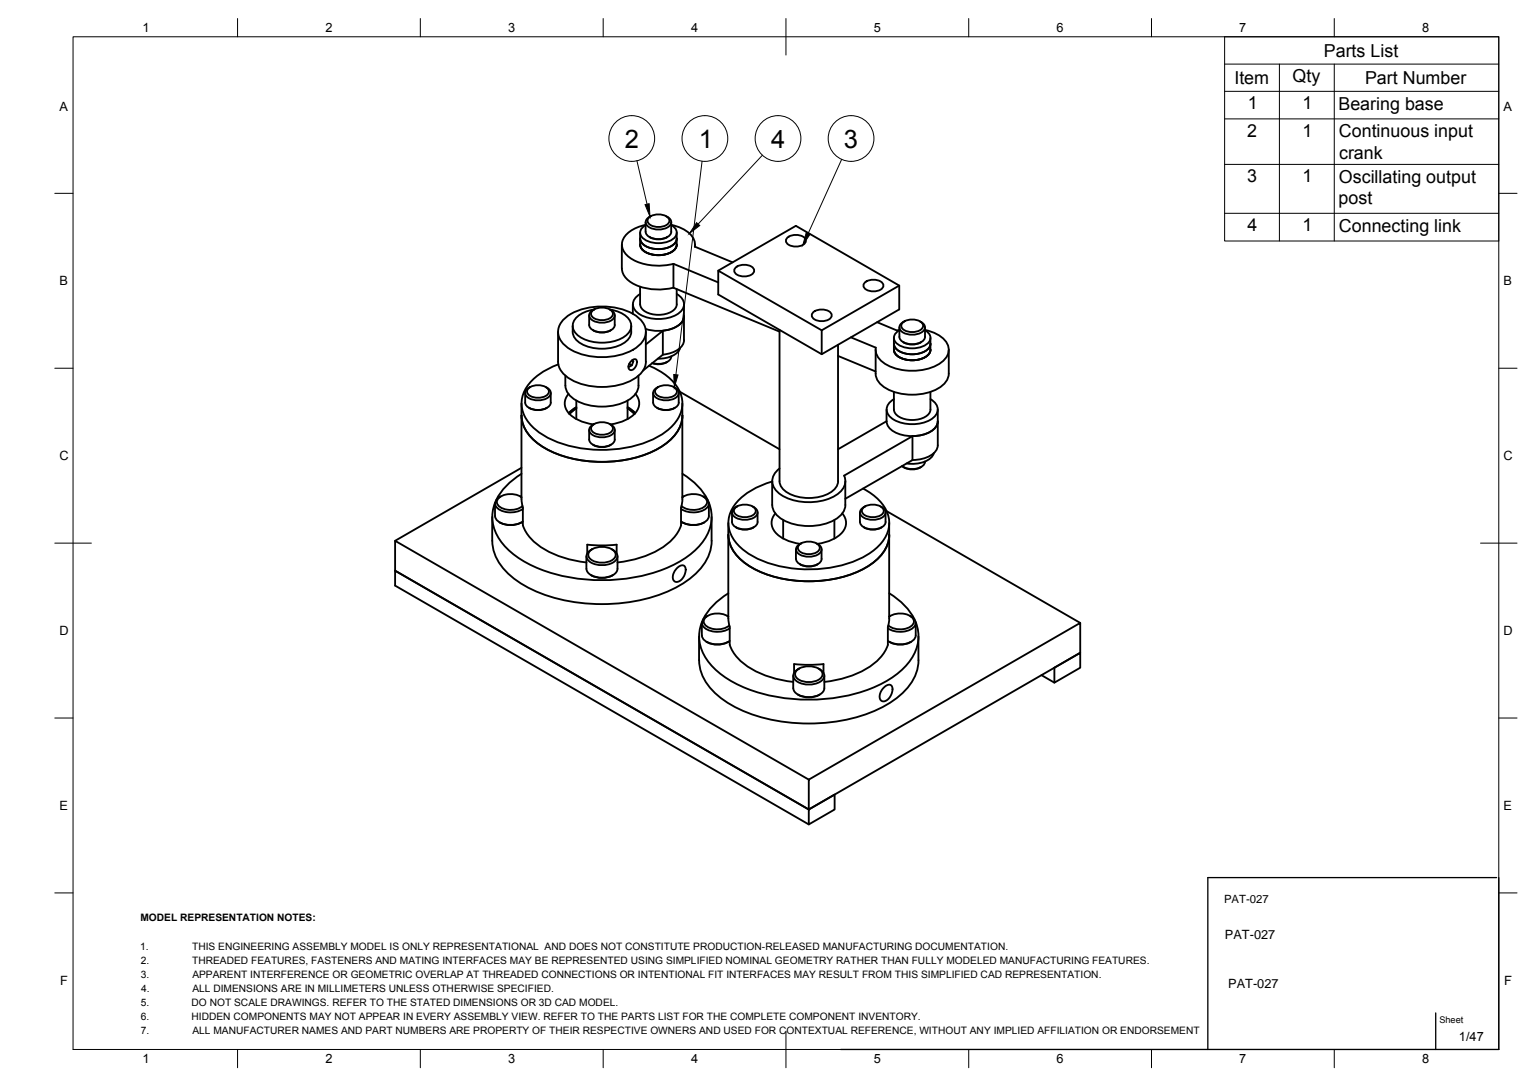
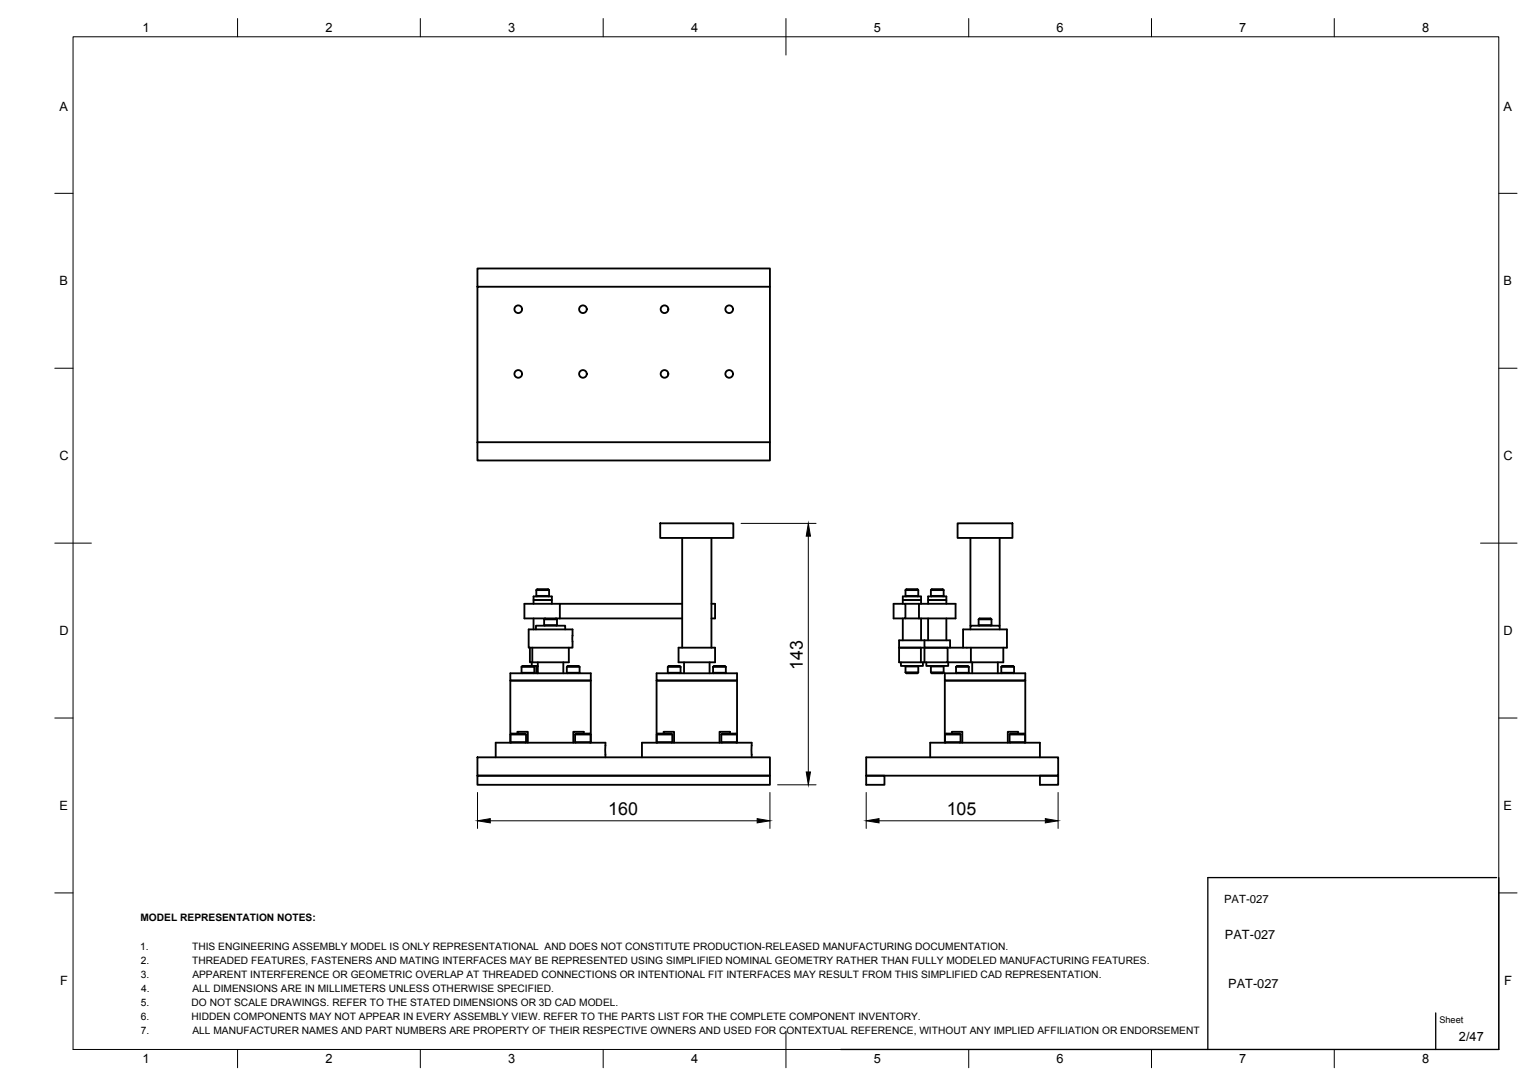
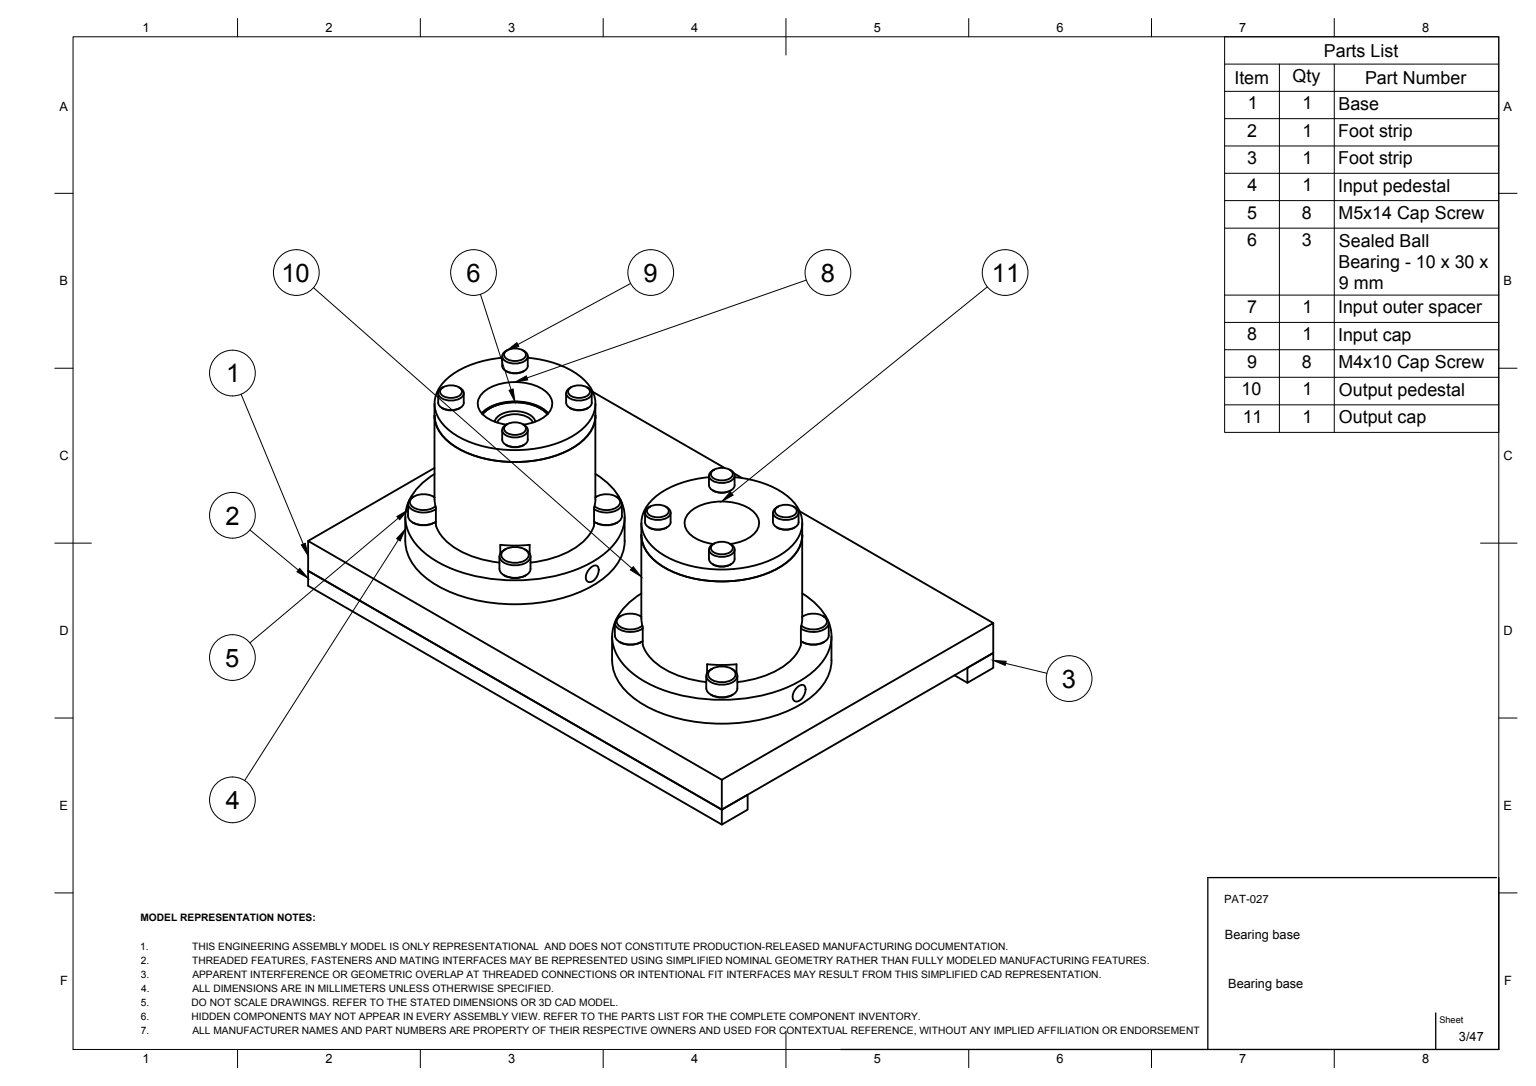
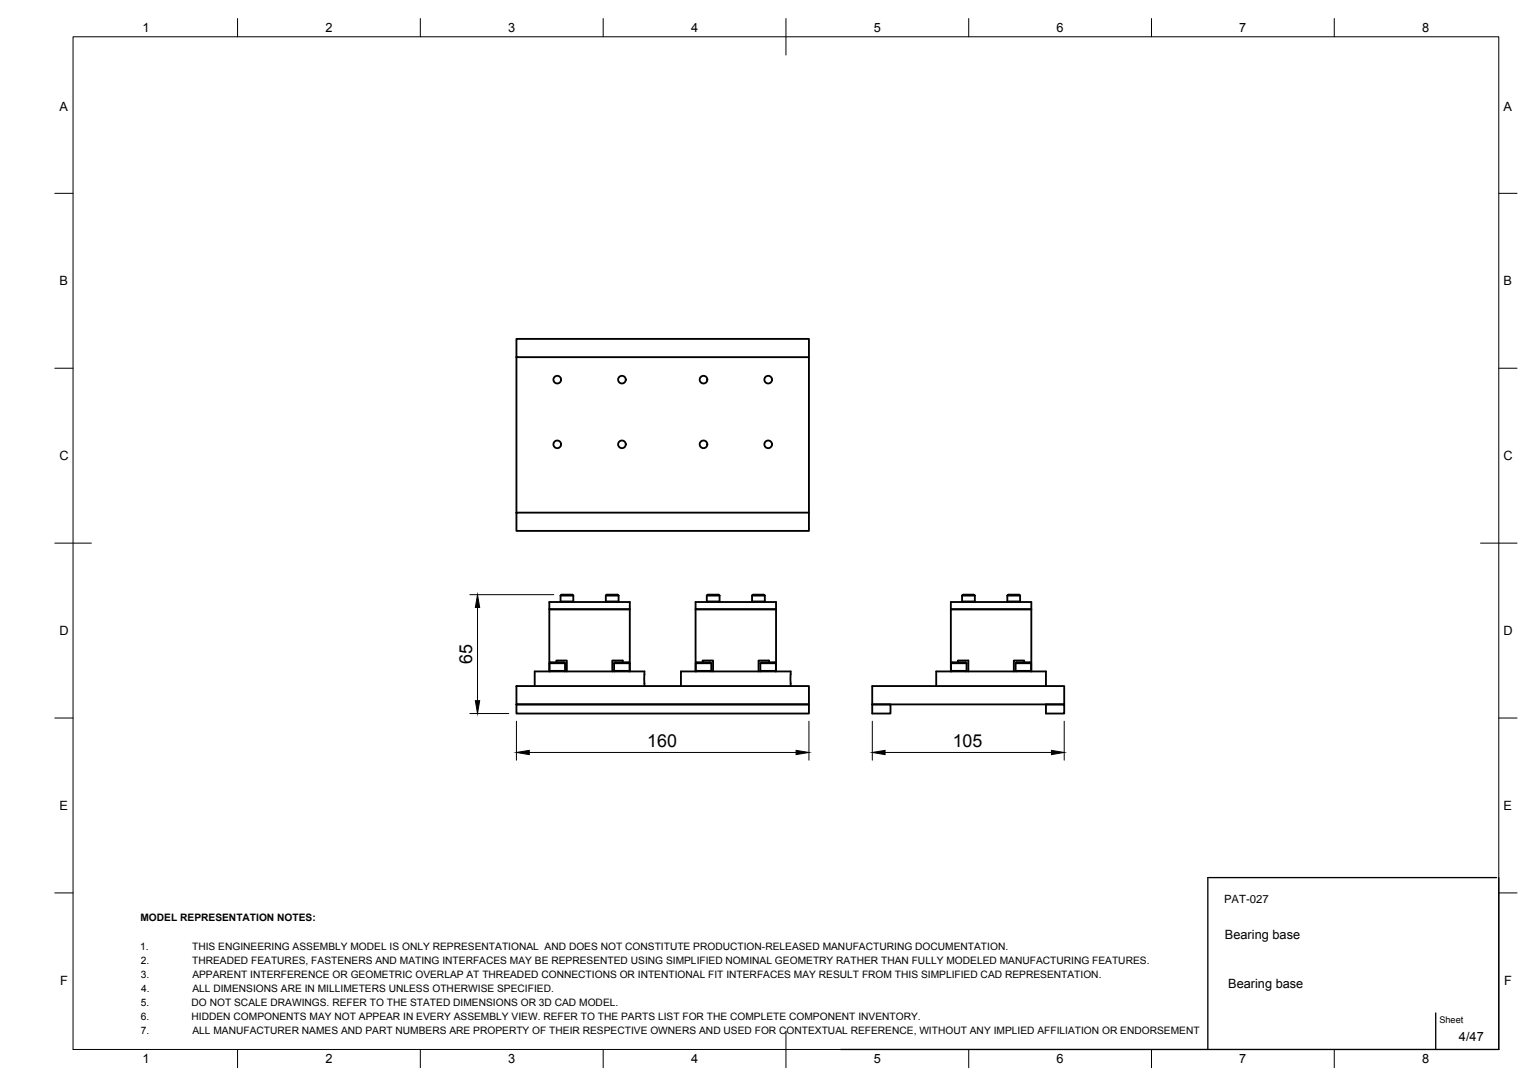
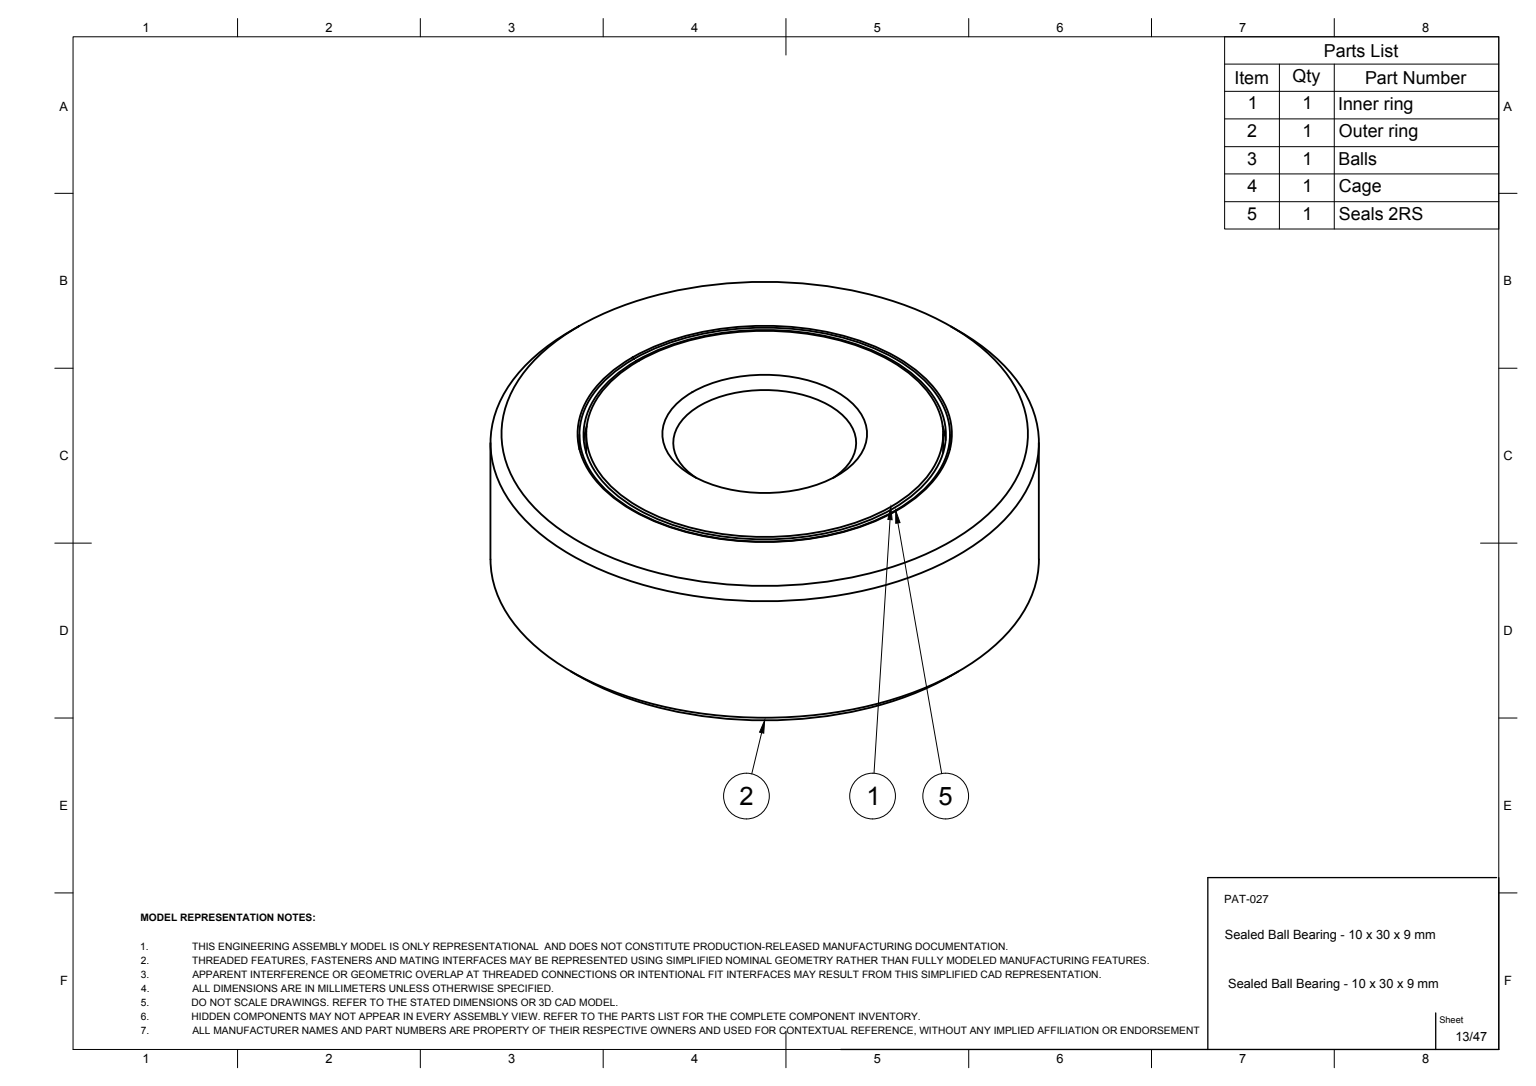
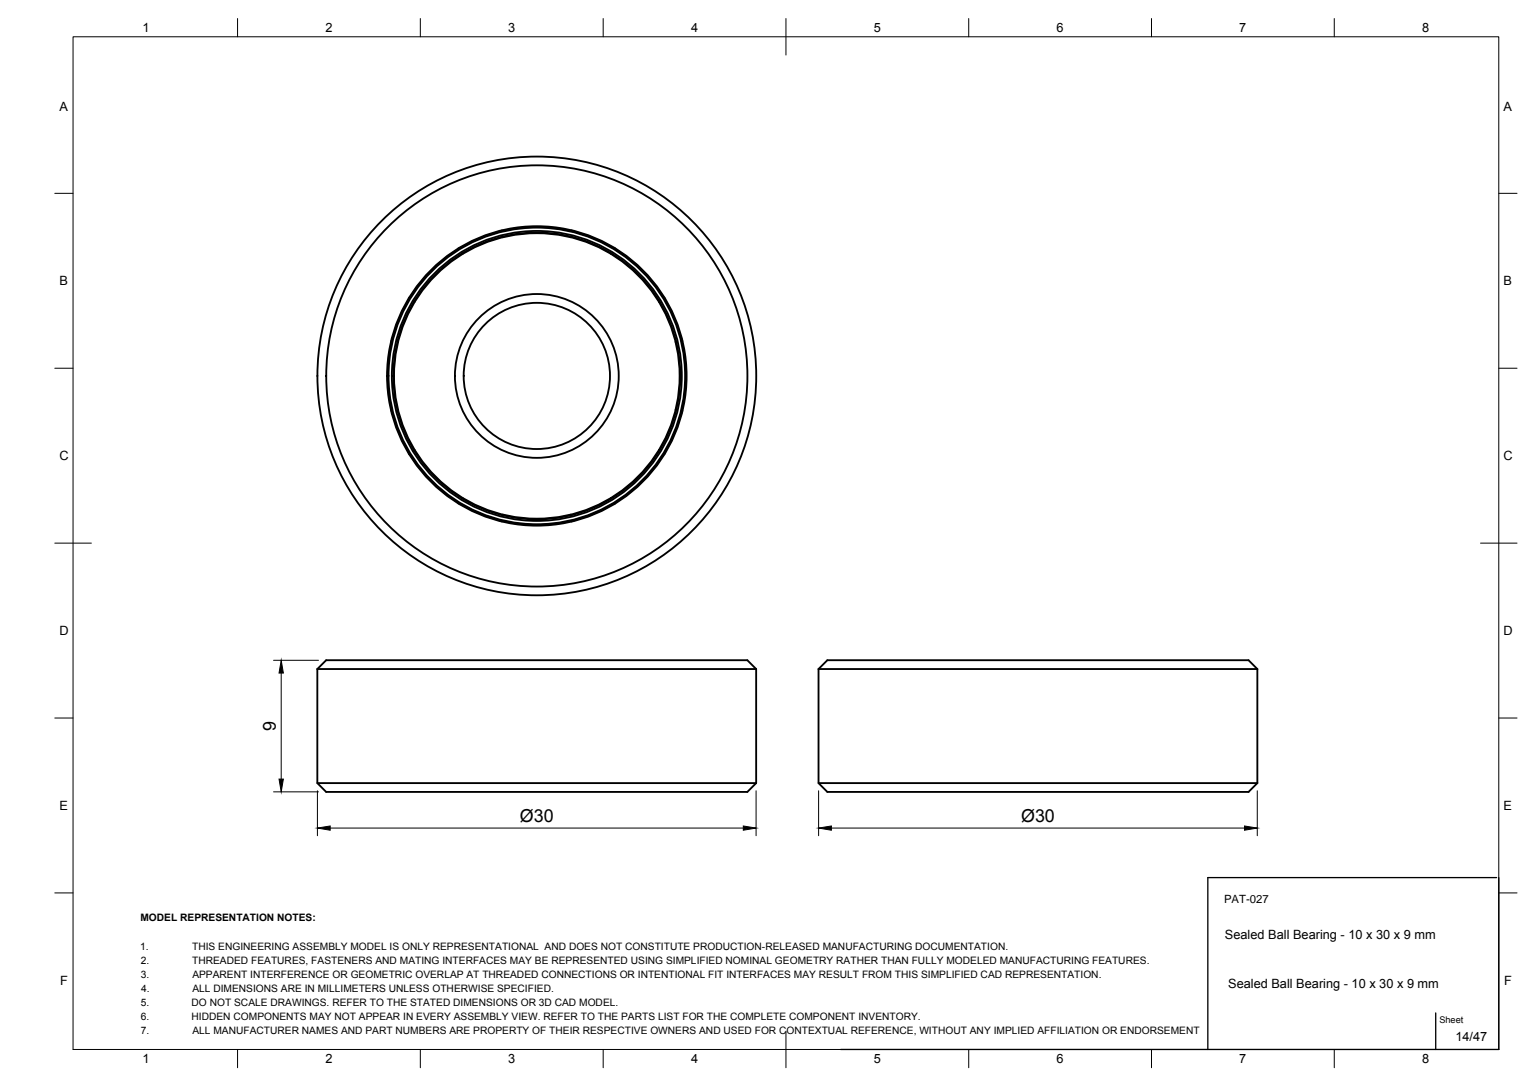
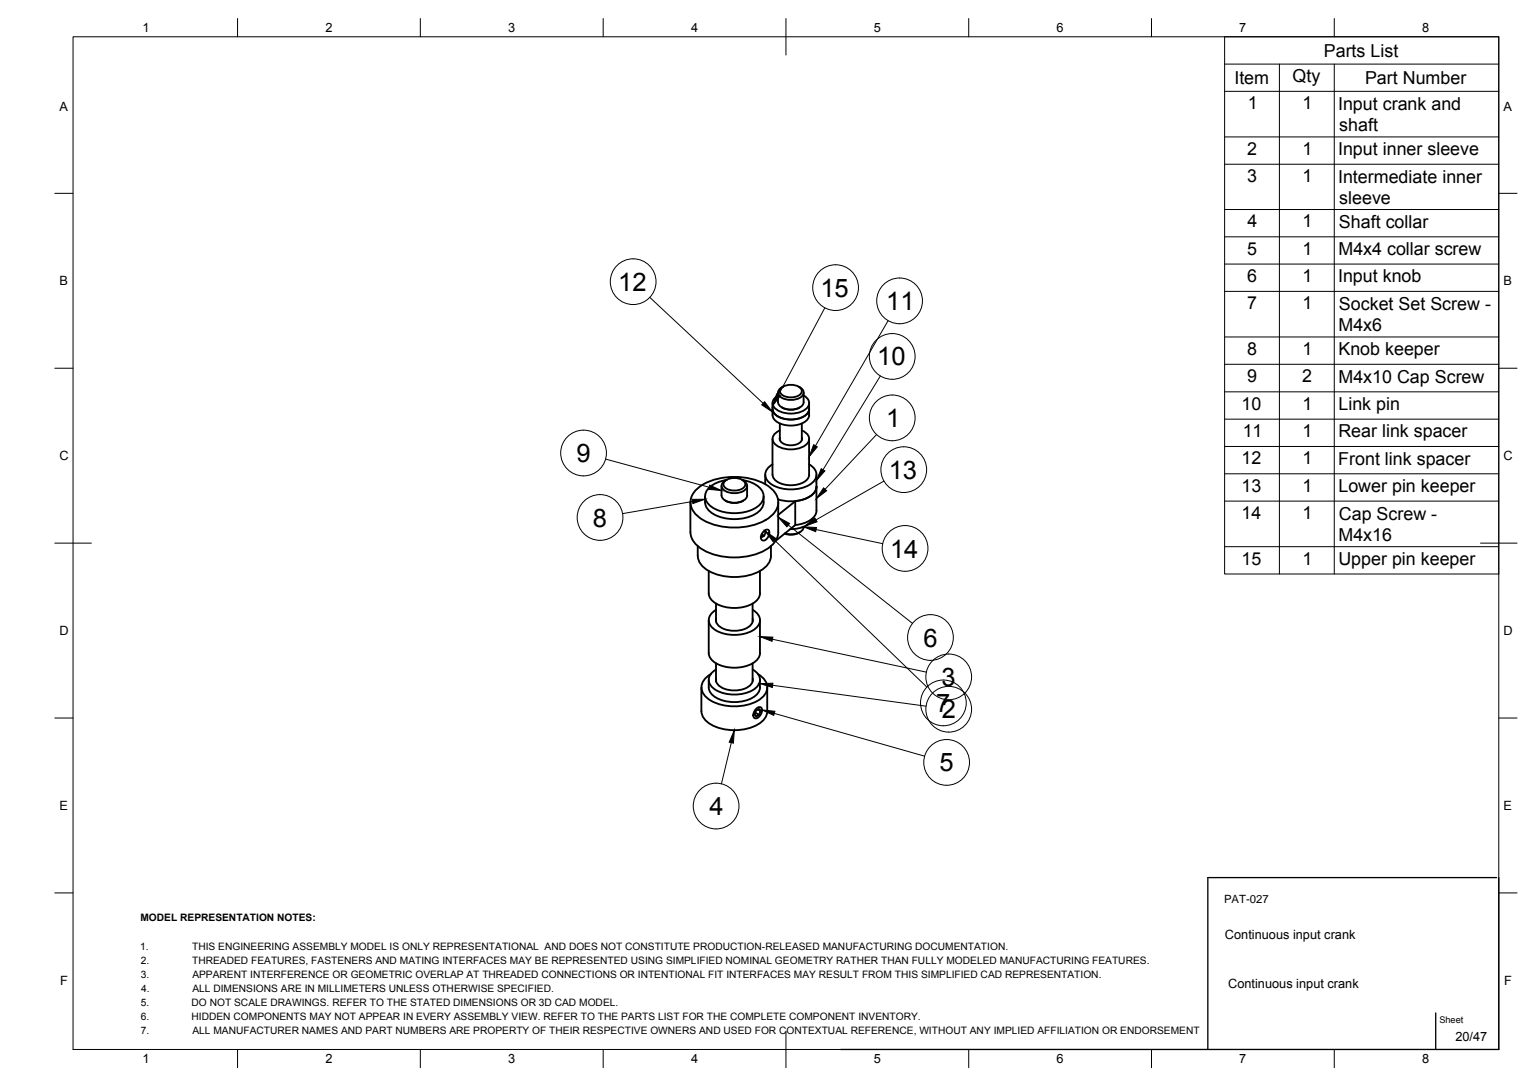
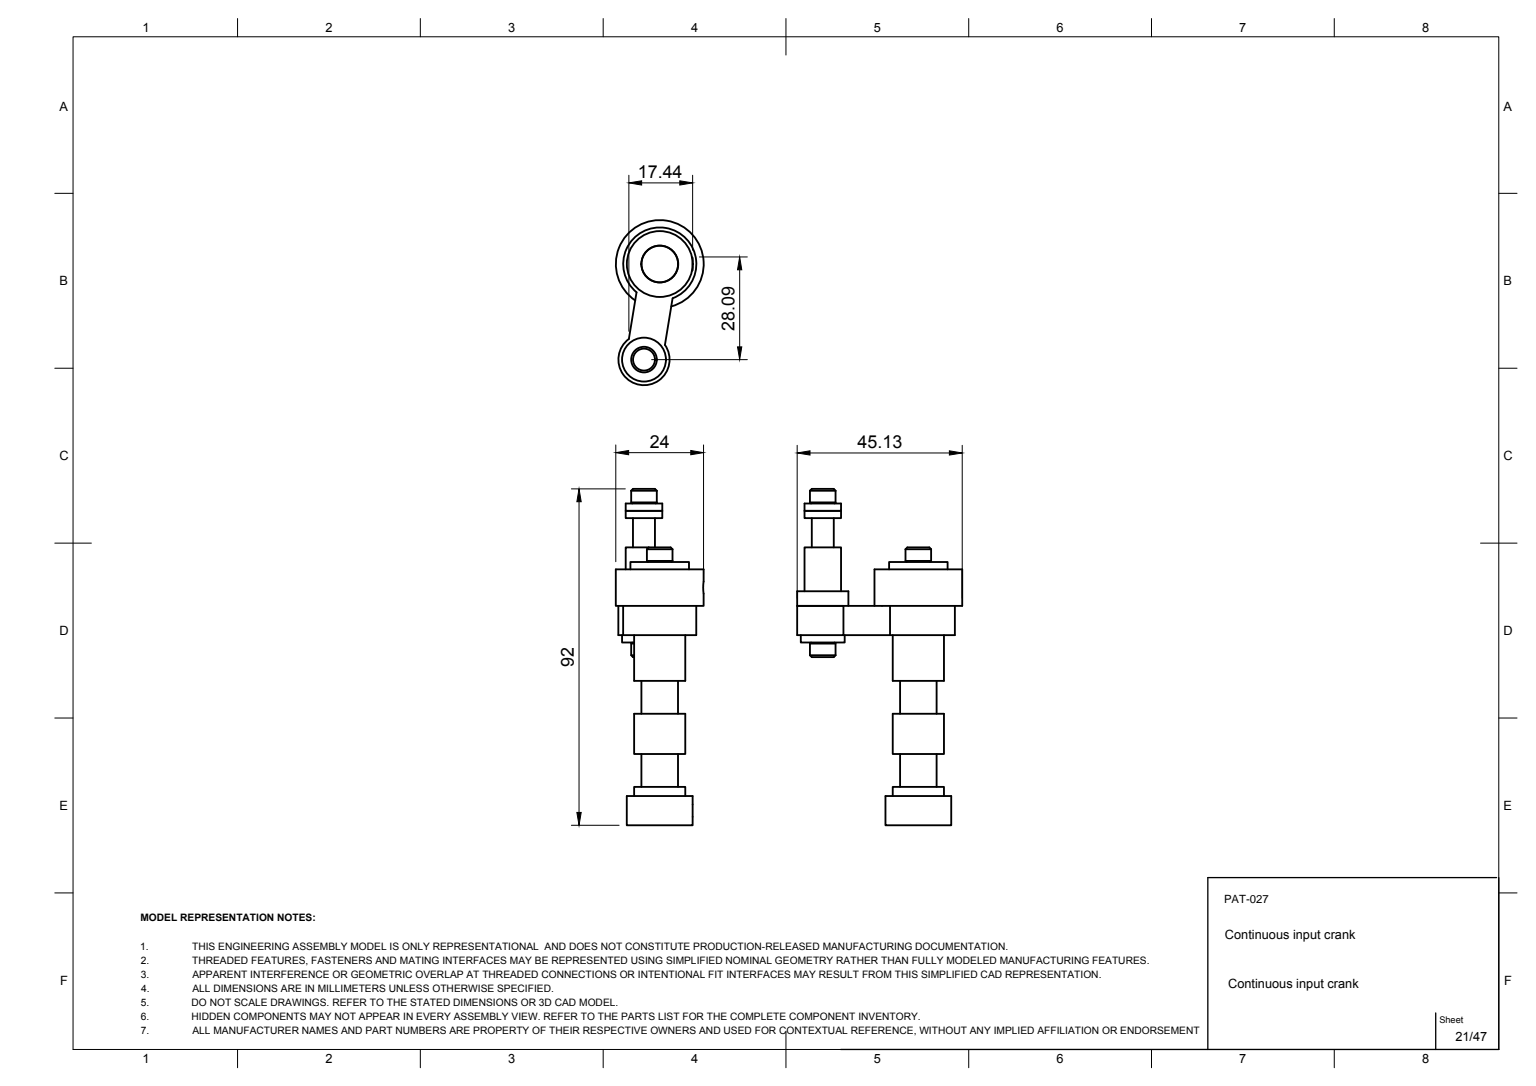
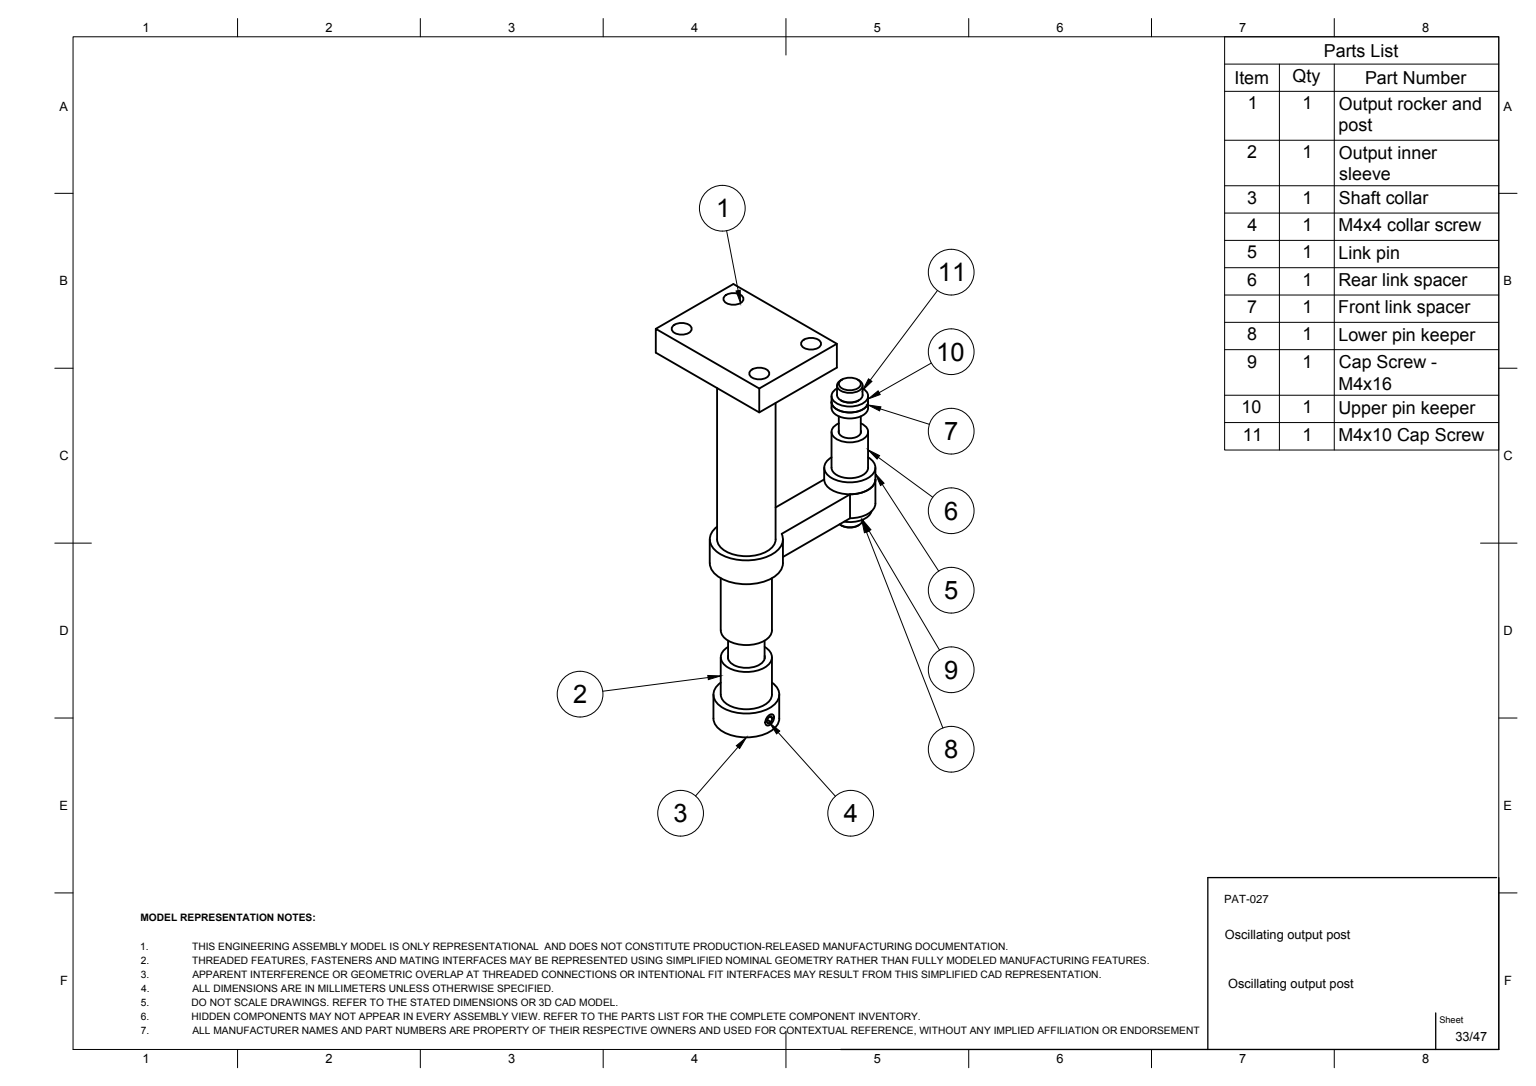
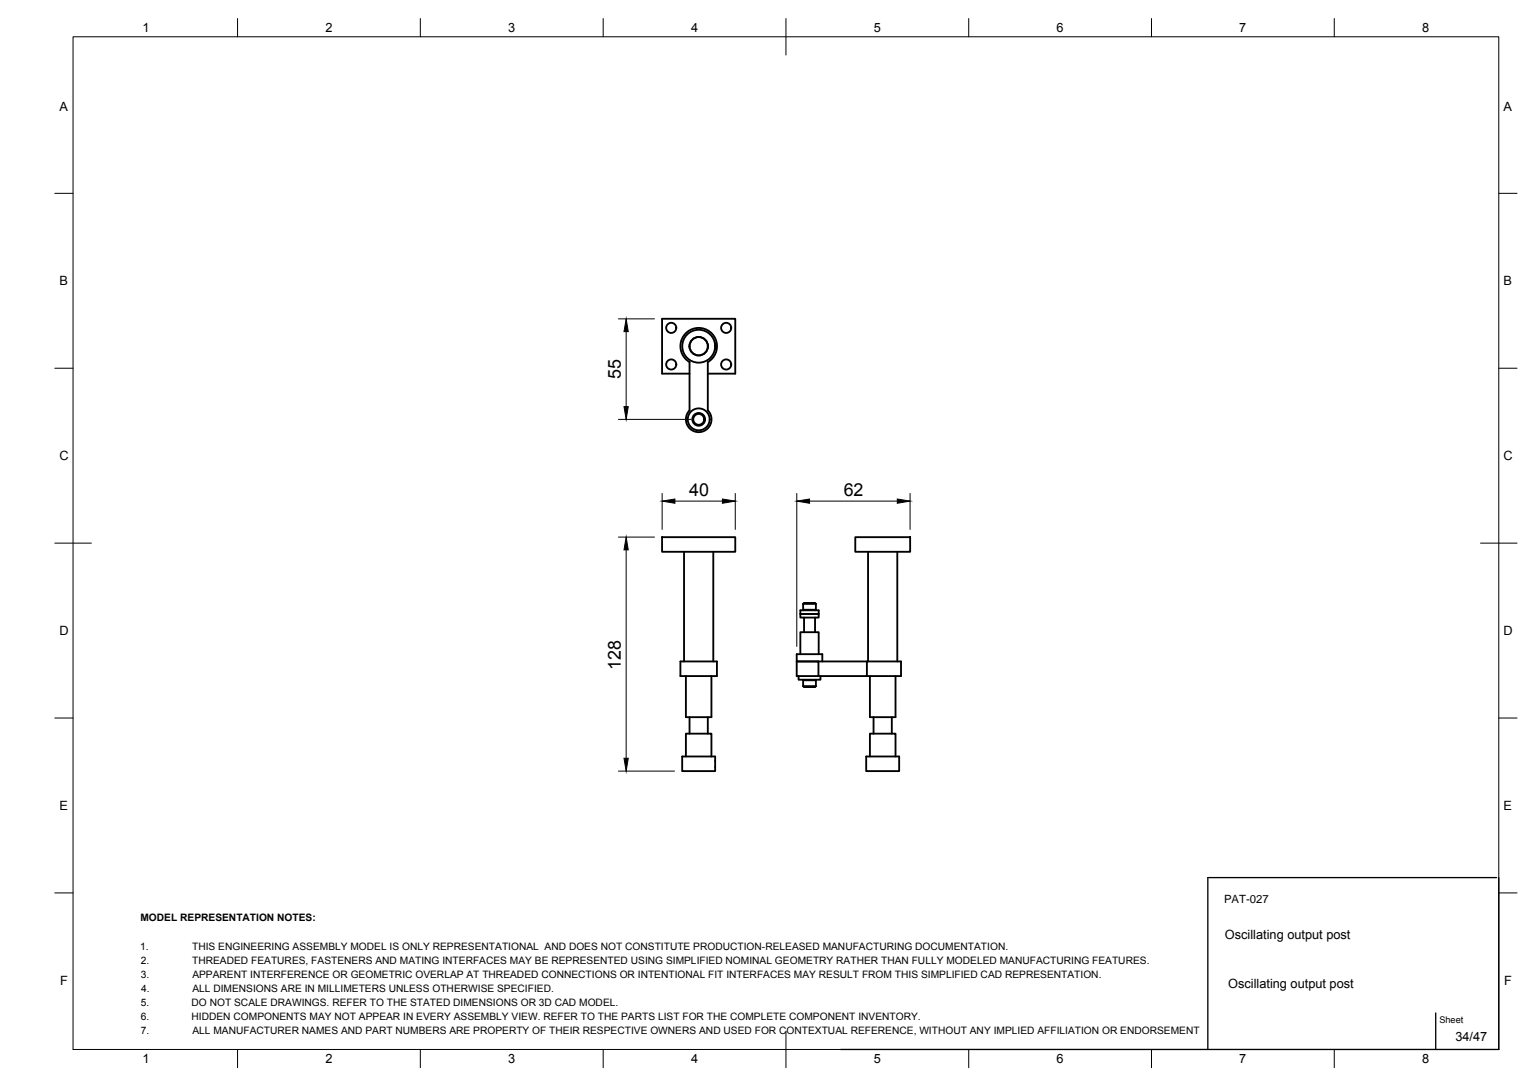
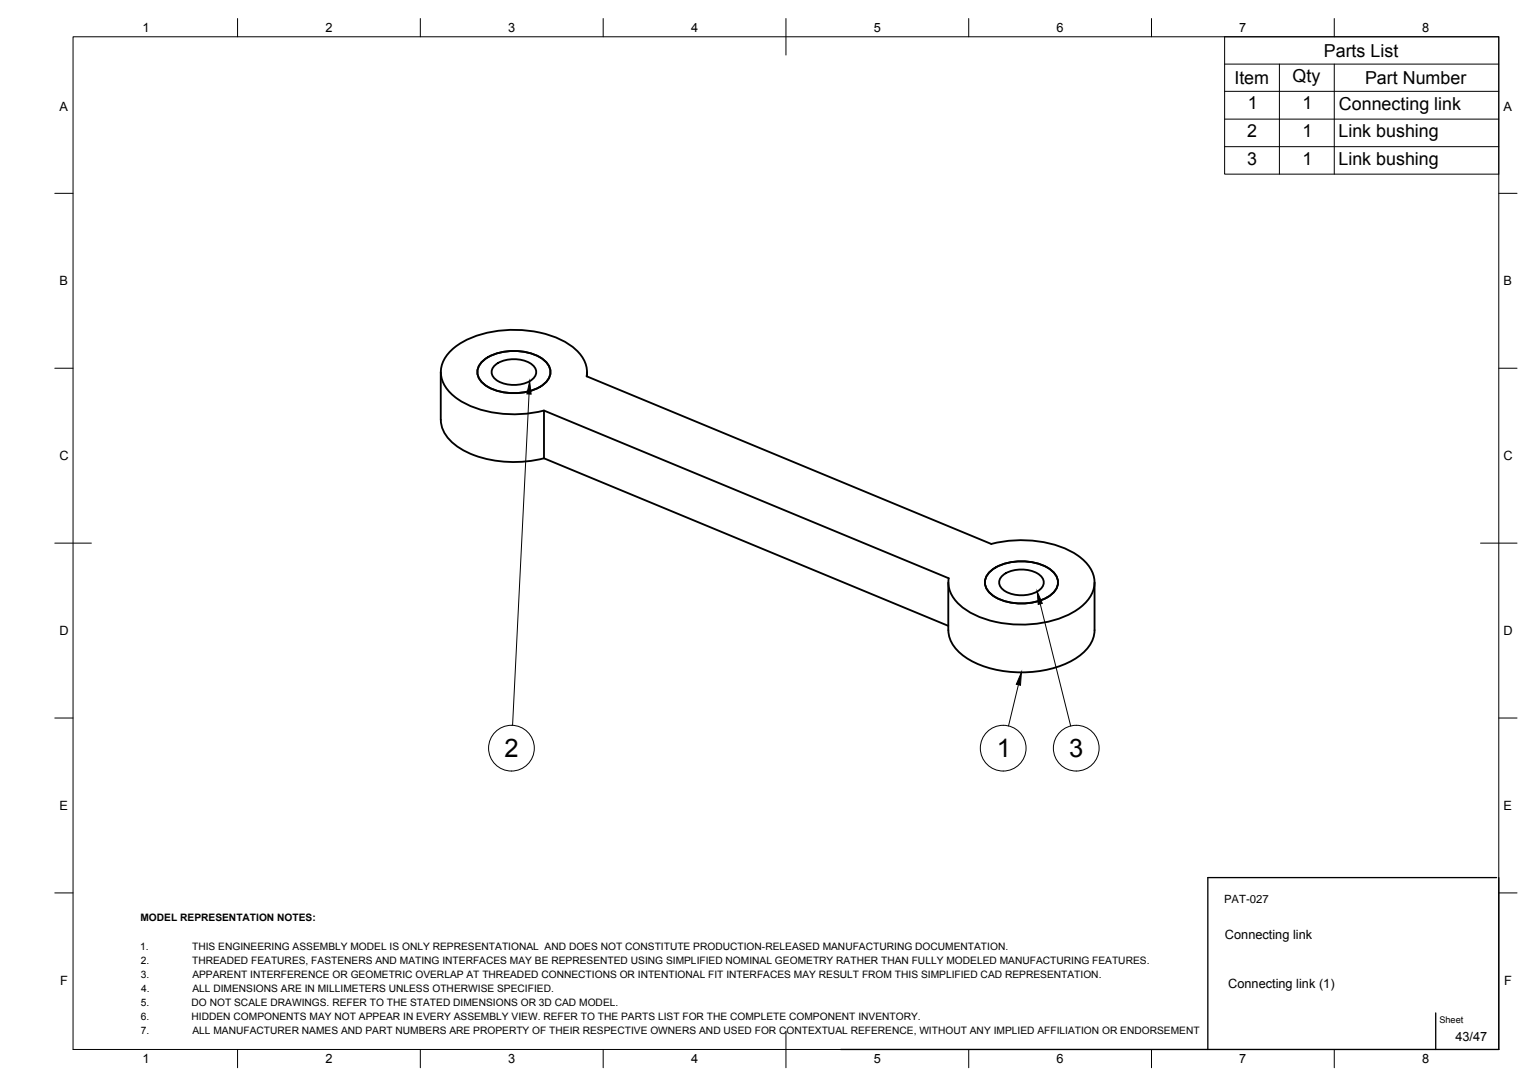
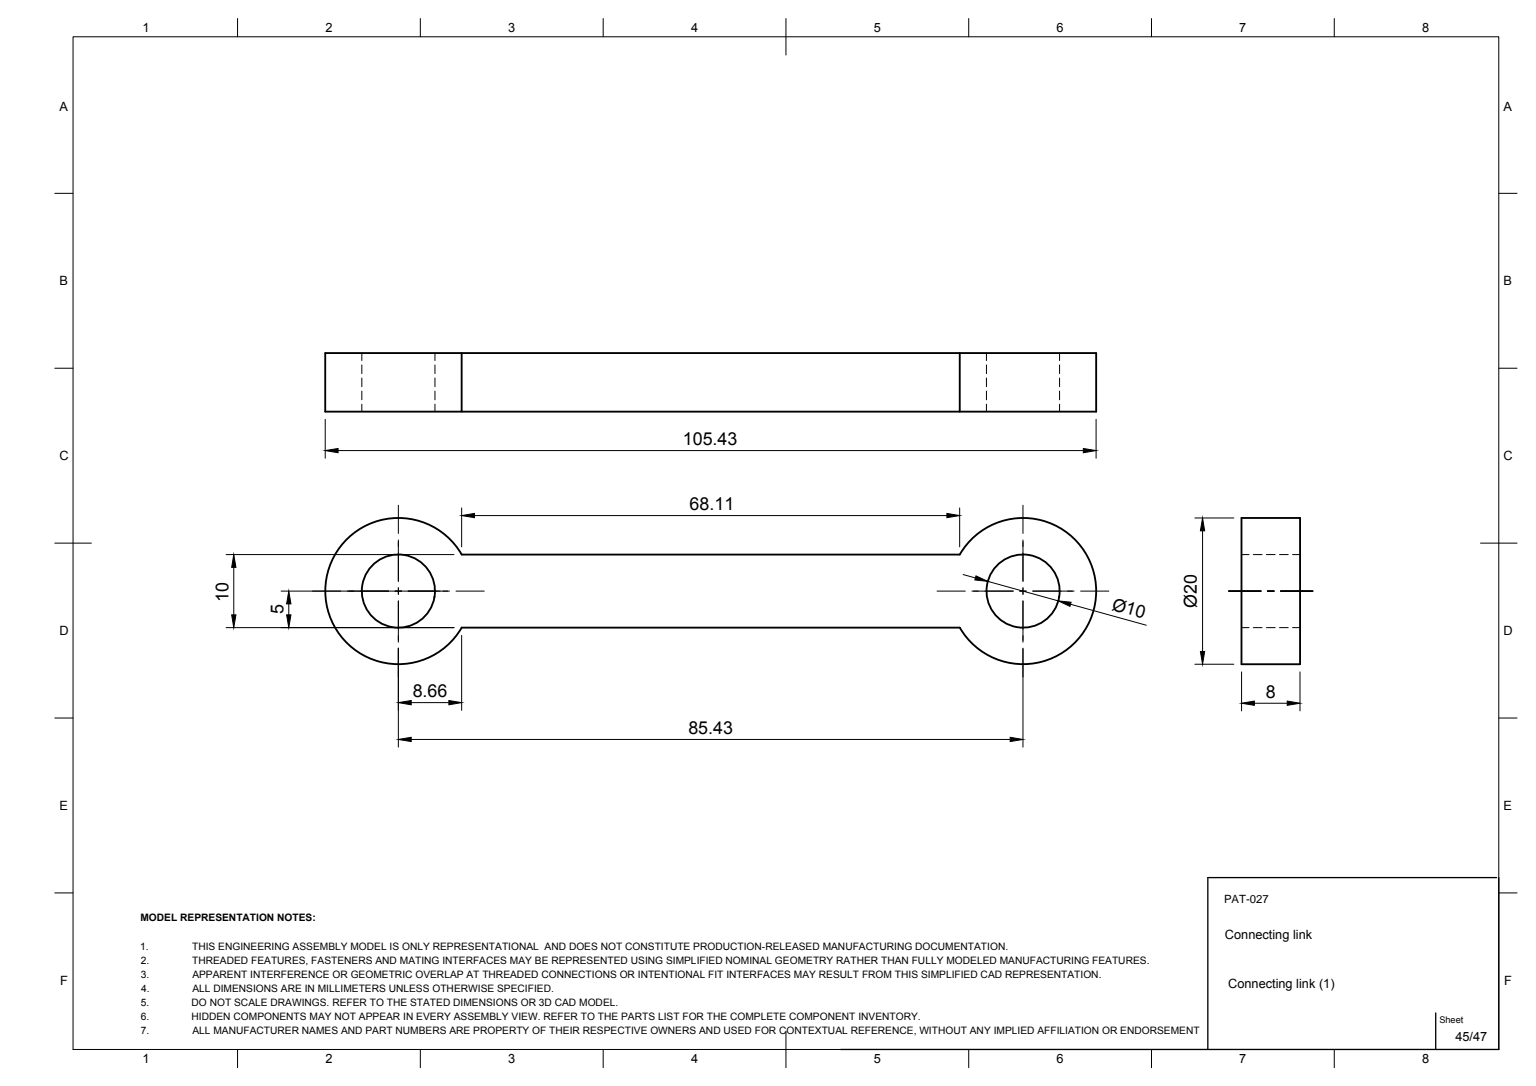
ISO-10303-21;
HEADER;
/* Generated by software containing ST-Developer
 * from STEP Tools, Inc. (www.steptools.com) 
 */

FILE_DESCRIPTION(
/* description */ ('Crank-driven oscillating fan base (mechanism only)'),

/* implementation_level */ '2;1');

FILE_NAME(
/* name */ 'PAT-027',
/* time_stamp */ '2026-10-28T03:25:00-07:00',
/* author */ (''),
/* organization */ (''),
/* preprocessor_version */ 'ST-DEVELOPER v20.2',
/* originating_system */ 'Autodesk Translation Framework v15.17.0.0',
/* authorisation */ '');

FILE_SCHEMA (('AUTOMOTIVE_DESIGN { 1 0 10303 214 3 1 1 }'));
ENDSEC;

DATA;
#10=MECHANICAL_DESIGN_GEOMETRIC_PRESENTATION_REPRESENTATION('',(#437,#438,
#439,#440,#441,#442,#443,#444,#445,#446,#447,#448,#449,#450,#451,#452,#453,
#454,#455,#456,#457,#458,#459,#460,#461,#462,#463,#464,#465,#466,#467,#468,
#469,#470,#471,#472,#473,#474,#475,#476,#477,#478,#479,#480,#481,#482,#483,
#484),#11916);
#11=ITEM_DEFINED_TRANSFORMATION($,$,#6830,#6958);
#12=ITEM_DEFINED_TRANSFORMATION($,$,#6850,#6959);
#13=ITEM_DEFINED_TRANSFORMATION($,$,#6870,#6960);
#14=ITEM_DEFINED_TRANSFORMATION($,$,#6887,#6961);
#15=ITEM_DEFINED_TRANSFORMATION($,$,#6941,#6962);
#16=ITEM_DEFINED_TRANSFORMATION($,$,#6561,#7314);
#17=ITEM_DEFINED_TRANSFORMATION($,$,#6592,#7315);
#18=ITEM_DEFINED_TRANSFORMATION($,$,#6599,#7316);
#19=ITEM_DEFINED_TRANSFORMATION($,$,#6606,#7317);
#20=ITEM_DEFINED_TRANSFORMATION($,$,#6676,#7318);
#21=ITEM_DEFINED_TRANSFORMATION($,$,#6685,#7319);
#22=ITEM_DEFINED_TRANSFORMATION($,$,#6710,#7320);
#23=ITEM_DEFINED_TRANSFORMATION($,$,#6780,#7321);
#24=ITEM_DEFINED_TRANSFORMATION($,$,#6805,#7322);
#25=ITEM_DEFINED_TRANSFORMATION($,$,#6805,#7323);
#26=ITEM_DEFINED_TRANSFORMATION($,$,#6805,#7324);
#27=ITEM_DEFINED_TRANSFORMATION($,$,#6805,#7325);
#28=ITEM_DEFINED_TRANSFORMATION($,$,#6829,#7326);
#29=ITEM_DEFINED_TRANSFORMATION($,$,#6829,#7327);
#30=ITEM_DEFINED_TRANSFORMATION($,$,#7290,#7328);
#31=ITEM_DEFINED_TRANSFORMATION($,$,#7290,#7329);
#32=ITEM_DEFINED_TRANSFORMATION($,$,#7290,#7330);
#33=ITEM_DEFINED_TRANSFORMATION($,$,#7290,#7331);
#34=ITEM_DEFINED_TRANSFORMATION($,$,#6805,#7332);
#35=ITEM_DEFINED_TRANSFORMATION($,$,#6805,#7333);
#36=ITEM_DEFINED_TRANSFORMATION($,$,#6805,#7334);
#37=ITEM_DEFINED_TRANSFORMATION($,$,#6805,#7335);
#38=ITEM_DEFINED_TRANSFORMATION($,$,#6829,#7336);
#39=ITEM_DEFINED_TRANSFORMATION($,$,#7290,#7337);
#40=ITEM_DEFINED_TRANSFORMATION($,$,#7290,#7338);
#41=ITEM_DEFINED_TRANSFORMATION($,$,#7290,#7339);
#42=ITEM_DEFINED_TRANSFORMATION($,$,#7290,#7340);
#43=ITEM_DEFINED_TRANSFORMATION($,$,#6964,#7341);
#44=ITEM_DEFINED_TRANSFORMATION($,$,#6994,#7342);
#45=ITEM_DEFINED_TRANSFORMATION($,$,#7003,#7343);
#46=ITEM_DEFINED_TRANSFORMATION($,$,#7012,#7344);
#47=ITEM_DEFINED_TRANSFORMATION($,$,#7026,#7345);
#48=ITEM_DEFINED_TRANSFORMATION($,$,#7040,#7346);
#49=ITEM_DEFINED_TRANSFORMATION($,$,#7049,#7347);
#50=ITEM_DEFINED_TRANSFORMATION($,$,#7071,#7348);
#51=ITEM_DEFINED_TRANSFORMATION($,$,#7080,#7349);
#52=ITEM_DEFINED_TRANSFORMATION($,$,#7089,#7350);
#53=ITEM_DEFINED_TRANSFORMATION($,$,#7098,#7351);
#54=ITEM_DEFINED_TRANSFORMATION($,$,#7249,#7352);
#55=ITEM_DEFINED_TRANSFORMATION($,$,#7107,#7353);
#56=ITEM_DEFINED_TRANSFORMATION($,$,#7290,#7354);
#57=ITEM_DEFINED_TRANSFORMATION($,$,#7264,#7355);
#58=ITEM_DEFINED_TRANSFORMATION($,$,#7290,#7356);
#59=ITEM_DEFINED_TRANSFORMATION($,$,#7125,#7357);
#60=ITEM_DEFINED_TRANSFORMATION($,$,#7168,#7358);
#61=ITEM_DEFINED_TRANSFORMATION($,$,#7177,#7359);
#62=ITEM_DEFINED_TRANSFORMATION($,$,#7191,#7360);
#63=ITEM_DEFINED_TRANSFORMATION($,$,#7213,#7361);
#64=ITEM_DEFINED_TRANSFORMATION($,$,#7222,#7362);
#65=ITEM_DEFINED_TRANSFORMATION($,$,#7231,#7363);
#66=ITEM_DEFINED_TRANSFORMATION($,$,#7240,#7364);
#67=ITEM_DEFINED_TRANSFORMATION($,$,#7249,#7365);
#68=ITEM_DEFINED_TRANSFORMATION($,$,#7264,#7366);
#69=ITEM_DEFINED_TRANSFORMATION($,$,#7290,#7367);
#70=ITEM_DEFINED_TRANSFORMATION($,$,#7369,#7404);
#71=ITEM_DEFINED_TRANSFORMATION($,$,#7386,#7405);
#72=ITEM_DEFINED_TRANSFORMATION($,$,#7395,#7406);
#73=ITEM_DEFINED_TRANSFORMATION($,$,#6560,#7407);
#74=ITEM_DEFINED_TRANSFORMATION($,$,#6963,#7408);
#75=ITEM_DEFINED_TRANSFORMATION($,$,#7124,#7409);
#76=ITEM_DEFINED_TRANSFORMATION($,$,#7368,#7410);
#77=(
REPRESENTATION_RELATIONSHIP($,$,#12091,#12090)
REPRESENTATION_RELATIONSHIP_WITH_TRANSFORMATION(#11)
SHAPE_REPRESENTATION_RELATIONSHIP()
);
#78=(
REPRESENTATION_RELATIONSHIP($,$,#12092,#12090)
REPRESENTATION_RELATIONSHIP_WITH_TRANSFORMATION(#12)
SHAPE_REPRESENTATION_RELATIONSHIP()
);
#79=(
REPRESENTATION_RELATIONSHIP($,$,#12093,#12090)
REPRESENTATION_RELATIONSHIP_WITH_TRANSFORMATION(#13)
SHAPE_REPRESENTATION_RELATIONSHIP()
);
#80=(
REPRESENTATION_RELATIONSHIP($,$,#12094,#12090)
REPRESENTATION_RELATIONSHIP_WITH_TRANSFORMATION(#14)
SHAPE_REPRESENTATION_RELATIONSHIP()
);
#81=(
REPRESENTATION_RELATIONSHIP($,$,#12095,#12090)
REPRESENTATION_RELATIONSHIP_WITH_TRANSFORMATION(#15)
SHAPE_REPRESENTATION_RELATIONSHIP()
);
#82=(
REPRESENTATION_RELATIONSHIP($,$,#12081,#12080)
REPRESENTATION_RELATIONSHIP_WITH_TRANSFORMATION(#16)
SHAPE_REPRESENTATION_RELATIONSHIP()
);
#83=(
REPRESENTATION_RELATIONSHIP($,$,#12082,#12080)
REPRESENTATION_RELATIONSHIP_WITH_TRANSFORMATION(#17)
SHAPE_REPRESENTATION_RELATIONSHIP()
);
#84=(
REPRESENTATION_RELATIONSHIP($,$,#12083,#12080)
REPRESENTATION_RELATIONSHIP_WITH_TRANSFORMATION(#18)
SHAPE_REPRESENTATION_RELATIONSHIP()
);
#85=(
REPRESENTATION_RELATIONSHIP($,$,#12084,#12080)
REPRESENTATION_RELATIONSHIP_WITH_TRANSFORMATION(#19)
SHAPE_REPRESENTATION_RELATIONSHIP()
);
#86=(
REPRESENTATION_RELATIONSHIP($,$,#12085,#12080)
REPRESENTATION_RELATIONSHIP_WITH_TRANSFORMATION(#20)
SHAPE_REPRESENTATION_RELATIONSHIP()
);
#87=(
REPRESENTATION_RELATIONSHIP($,$,#12086,#12080)
REPRESENTATION_RELATIONSHIP_WITH_TRANSFORMATION(#21)
SHAPE_REPRESENTATION_RELATIONSHIP()
);
#88=(
REPRESENTATION_RELATIONSHIP($,$,#12087,#12080)
REPRESENTATION_RELATIONSHIP_WITH_TRANSFORMATION(#22)
SHAPE_REPRESENTATION_RELATIONSHIP()
);
#89=(
REPRESENTATION_RELATIONSHIP($,$,#12088,#12080)
REPRESENTATION_RELATIONSHIP_WITH_TRANSFORMATION(#23)
SHAPE_REPRESENTATION_RELATIONSHIP()
);
#90=(
REPRESENTATION_RELATIONSHIP($,$,#12089,#12080)
REPRESENTATION_RELATIONSHIP_WITH_TRANSFORMATION(#24)
SHAPE_REPRESENTATION_RELATIONSHIP()
);
#91=(
REPRESENTATION_RELATIONSHIP($,$,#12089,#12080)
REPRESENTATION_RELATIONSHIP_WITH_TRANSFORMATION(#25)
SHAPE_REPRESENTATION_RELATIONSHIP()
);
#92=(
REPRESENTATION_RELATIONSHIP($,$,#12089,#12080)
REPRESENTATION_RELATIONSHIP_WITH_TRANSFORMATION(#26)
SHAPE_REPRESENTATION_RELATIONSHIP()
);
#93=(
REPRESENTATION_RELATIONSHIP($,$,#12089,#12080)
REPRESENTATION_RELATIONSHIP_WITH_TRANSFORMATION(#27)
SHAPE_REPRESENTATION_RELATIONSHIP()
);
#94=(
REPRESENTATION_RELATIONSHIP($,$,#12090,#12080)
REPRESENTATION_RELATIONSHIP_WITH_TRANSFORMATION(#28)
SHAPE_REPRESENTATION_RELATIONSHIP()
);
#95=(
REPRESENTATION_RELATIONSHIP($,$,#12090,#12080)
REPRESENTATION_RELATIONSHIP_WITH_TRANSFORMATION(#29)
SHAPE_REPRESENTATION_RELATIONSHIP()
);
#96=(
REPRESENTATION_RELATIONSHIP($,$,#12120,#12080)
REPRESENTATION_RELATIONSHIP_WITH_TRANSFORMATION(#30)
SHAPE_REPRESENTATION_RELATIONSHIP()
);
#97=(
REPRESENTATION_RELATIONSHIP($,$,#12120,#12080)
REPRESENTATION_RELATIONSHIP_WITH_TRANSFORMATION(#31)
SHAPE_REPRESENTATION_RELATIONSHIP()
);
#98=(
REPRESENTATION_RELATIONSHIP($,$,#12120,#12080)
REPRESENTATION_RELATIONSHIP_WITH_TRANSFORMATION(#32)
SHAPE_REPRESENTATION_RELATIONSHIP()
);
#99=(
REPRESENTATION_RELATIONSHIP($,$,#12120,#12080)
REPRESENTATION_RELATIONSHIP_WITH_TRANSFORMATION(#33)
SHAPE_REPRESENTATION_RELATIONSHIP()
);
#100=(
REPRESENTATION_RELATIONSHIP($,$,#12089,#12080)
REPRESENTATION_RELATIONSHIP_WITH_TRANSFORMATION(#34)
SHAPE_REPRESENTATION_RELATIONSHIP()
);
#101=(
REPRESENTATION_RELATIONSHIP($,$,#12089,#12080)
REPRESENTATION_RELATIONSHIP_WITH_TRANSFORMATION(#35)
SHAPE_REPRESENTATION_RELATIONSHIP()
);
#102=(
REPRESENTATION_RELATIONSHIP($,$,#12089,#12080)
REPRESENTATION_RELATIONSHIP_WITH_TRANSFORMATION(#36)
SHAPE_REPRESENTATION_RELATIONSHIP()
);
#103=(
REPRESENTATION_RELATIONSHIP($,$,#12089,#12080)
REPRESENTATION_RELATIONSHIP_WITH_TRANSFORMATION(#37)
SHAPE_REPRESENTATION_RELATIONSHIP()
);
#104=(
REPRESENTATION_RELATIONSHIP($,$,#12090,#12080)
REPRESENTATION_RELATIONSHIP_WITH_TRANSFORMATION(#38)
SHAPE_REPRESENTATION_RELATIONSHIP()
);
#105=(
REPRESENTATION_RELATIONSHIP($,$,#12120,#12080)
REPRESENTATION_RELATIONSHIP_WITH_TRANSFORMATION(#39)
SHAPE_REPRESENTATION_RELATIONSHIP()
);
#106=(
REPRESENTATION_RELATIONSHIP($,$,#12120,#12080)
REPRESENTATION_RELATIONSHIP_WITH_TRANSFORMATION(#40)
SHAPE_REPRESENTATION_RELATIONSHIP()
);
#107=(
REPRESENTATION_RELATIONSHIP($,$,#12120,#12080)
REPRESENTATION_RELATIONSHIP_WITH_TRANSFORMATION(#41)
SHAPE_REPRESENTATION_RELATIONSHIP()
);
#108=(
REPRESENTATION_RELATIONSHIP($,$,#12120,#12080)
REPRESENTATION_RELATIONSHIP_WITH_TRANSFORMATION(#42)
SHAPE_REPRESENTATION_RELATIONSHIP()
);
#109=(
REPRESENTATION_RELATIONSHIP($,$,#12097,#12096)
REPRESENTATION_RELATIONSHIP_WITH_TRANSFORMATION(#43)
SHAPE_REPRESENTATION_RELATIONSHIP()
);
#110=(
REPRESENTATION_RELATIONSHIP($,$,#12098,#12096)
REPRESENTATION_RELATIONSHIP_WITH_TRANSFORMATION(#44)
SHAPE_REPRESENTATION_RELATIONSHIP()
);
#111=(
REPRESENTATION_RELATIONSHIP($,$,#12099,#12096)
REPRESENTATION_RELATIONSHIP_WITH_TRANSFORMATION(#45)
SHAPE_REPRESENTATION_RELATIONSHIP()
);
#112=(
REPRESENTATION_RELATIONSHIP($,$,#12100,#12096)
REPRESENTATION_RELATIONSHIP_WITH_TRANSFORMATION(#46)
SHAPE_REPRESENTATION_RELATIONSHIP()
);
#113=(
REPRESENTATION_RELATIONSHIP($,$,#12101,#12096)
REPRESENTATION_RELATIONSHIP_WITH_TRANSFORMATION(#47)
SHAPE_REPRESENTATION_RELATIONSHIP()
);
#114=(
REPRESENTATION_RELATIONSHIP($,$,#12102,#12096)
REPRESENTATION_RELATIONSHIP_WITH_TRANSFORMATION(#48)
SHAPE_REPRESENTATION_RELATIONSHIP()
);
#115=(
REPRESENTATION_RELATIONSHIP($,$,#12103,#12096)
REPRESENTATION_RELATIONSHIP_WITH_TRANSFORMATION(#49)
SHAPE_REPRESENTATION_RELATIONSHIP()
);
#116=(
REPRESENTATION_RELATIONSHIP($,$,#12104,#12096)
REPRESENTATION_RELATIONSHIP_WITH_TRANSFORMATION(#50)
SHAPE_REPRESENTATION_RELATIONSHIP()
);
#117=(
REPRESENTATION_RELATIONSHIP($,$,#12105,#12096)
REPRESENTATION_RELATIONSHIP_WITH_TRANSFORMATION(#51)
SHAPE_REPRESENTATION_RELATIONSHIP()
);
#118=(
REPRESENTATION_RELATIONSHIP($,$,#12106,#12096)
REPRESENTATION_RELATIONSHIP_WITH_TRANSFORMATION(#52)
SHAPE_REPRESENTATION_RELATIONSHIP()
);
#119=(
REPRESENTATION_RELATIONSHIP($,$,#12107,#12096)
REPRESENTATION_RELATIONSHIP_WITH_TRANSFORMATION(#53)
SHAPE_REPRESENTATION_RELATIONSHIP()
);
#120=(
REPRESENTATION_RELATIONSHIP($,$,#12118,#12096)
REPRESENTATION_RELATIONSHIP_WITH_TRANSFORMATION(#54)
SHAPE_REPRESENTATION_RELATIONSHIP()
);
#121=(
REPRESENTATION_RELATIONSHIP($,$,#12108,#12096)
REPRESENTATION_RELATIONSHIP_WITH_TRANSFORMATION(#55)
SHAPE_REPRESENTATION_RELATIONSHIP()
);
#122=(
REPRESENTATION_RELATIONSHIP($,$,#12120,#12096)
REPRESENTATION_RELATIONSHIP_WITH_TRANSFORMATION(#56)
SHAPE_REPRESENTATION_RELATIONSHIP()
);
#123=(
REPRESENTATION_RELATIONSHIP($,$,#12119,#12096)
REPRESENTATION_RELATIONSHIP_WITH_TRANSFORMATION(#57)
SHAPE_REPRESENTATION_RELATIONSHIP()
);
#124=(
REPRESENTATION_RELATIONSHIP($,$,#12120,#12096)
REPRESENTATION_RELATIONSHIP_WITH_TRANSFORMATION(#58)
SHAPE_REPRESENTATION_RELATIONSHIP()
);
#125=(
REPRESENTATION_RELATIONSHIP($,$,#12110,#12109)
REPRESENTATION_RELATIONSHIP_WITH_TRANSFORMATION(#59)
SHAPE_REPRESENTATION_RELATIONSHIP()
);
#126=(
REPRESENTATION_RELATIONSHIP($,$,#12111,#12109)
REPRESENTATION_RELATIONSHIP_WITH_TRANSFORMATION(#60)
SHAPE_REPRESENTATION_RELATIONSHIP()
);
#127=(
REPRESENTATION_RELATIONSHIP($,$,#12112,#12109)
REPRESENTATION_RELATIONSHIP_WITH_TRANSFORMATION(#61)
SHAPE_REPRESENTATION_RELATIONSHIP()
);
#128=(
REPRESENTATION_RELATIONSHIP($,$,#12113,#12109)
REPRESENTATION_RELATIONSHIP_WITH_TRANSFORMATION(#62)
SHAPE_REPRESENTATION_RELATIONSHIP()
);
#129=(
REPRESENTATION_RELATIONSHIP($,$,#12114,#12109)
REPRESENTATION_RELATIONSHIP_WITH_TRANSFORMATION(#63)
SHAPE_REPRESENTATION_RELATIONSHIP()
);
#130=(
REPRESENTATION_RELATIONSHIP($,$,#12115,#12109)
REPRESENTATION_RELATIONSHIP_WITH_TRANSFORMATION(#64)
SHAPE_REPRESENTATION_RELATIONSHIP()
);
#131=(
REPRESENTATION_RELATIONSHIP($,$,#12116,#12109)
REPRESENTATION_RELATIONSHIP_WITH_TRANSFORMATION(#65)
SHAPE_REPRESENTATION_RELATIONSHIP()
);
#132=(
REPRESENTATION_RELATIONSHIP($,$,#12117,#12109)
REPRESENTATION_RELATIONSHIP_WITH_TRANSFORMATION(#66)
SHAPE_REPRESENTATION_RELATIONSHIP()
);
#133=(
REPRESENTATION_RELATIONSHIP($,$,#12118,#12109)
REPRESENTATION_RELATIONSHIP_WITH_TRANSFORMATION(#67)
SHAPE_REPRESENTATION_RELATIONSHIP()
);
#134=(
REPRESENTATION_RELATIONSHIP($,$,#12119,#12109)
REPRESENTATION_RELATIONSHIP_WITH_TRANSFORMATION(#68)
SHAPE_REPRESENTATION_RELATIONSHIP()
);
#135=(
REPRESENTATION_RELATIONSHIP($,$,#12120,#12109)
REPRESENTATION_RELATIONSHIP_WITH_TRANSFORMATION(#69)
SHAPE_REPRESENTATION_RELATIONSHIP()
);
#136=(
REPRESENTATION_RELATIONSHIP($,$,#12122,#12121)
REPRESENTATION_RELATIONSHIP_WITH_TRANSFORMATION(#70)
SHAPE_REPRESENTATION_RELATIONSHIP()
);
#137=(
REPRESENTATION_RELATIONSHIP($,$,#12123,#12121)
REPRESENTATION_RELATIONSHIP_WITH_TRANSFORMATION(#71)
SHAPE_REPRESENTATION_RELATIONSHIP()
);
#138=(
REPRESENTATION_RELATIONSHIP($,$,#12124,#12121)
REPRESENTATION_RELATIONSHIP_WITH_TRANSFORMATION(#72)
SHAPE_REPRESENTATION_RELATIONSHIP()
);
#139=(
REPRESENTATION_RELATIONSHIP($,$,#12080,#12079)
REPRESENTATION_RELATIONSHIP_WITH_TRANSFORMATION(#73)
SHAPE_REPRESENTATION_RELATIONSHIP()
);
#140=(
REPRESENTATION_RELATIONSHIP($,$,#12096,#12079)
REPRESENTATION_RELATIONSHIP_WITH_TRANSFORMATION(#74)
SHAPE_REPRESENTATION_RELATIONSHIP()
);
#141=(
REPRESENTATION_RELATIONSHIP($,$,#12109,#12079)
REPRESENTATION_RELATIONSHIP_WITH_TRANSFORMATION(#75)
SHAPE_REPRESENTATION_RELATIONSHIP()
);
#142=(
REPRESENTATION_RELATIONSHIP($,$,#12121,#12079)
REPRESENTATION_RELATIONSHIP_WITH_TRANSFORMATION(#76)
SHAPE_REPRESENTATION_RELATIONSHIP()
);
#143=CONTEXT_DEPENDENT_SHAPE_REPRESENTATION(#77,#11984);
#144=CONTEXT_DEPENDENT_SHAPE_REPRESENTATION(#78,#11985);
#145=CONTEXT_DEPENDENT_SHAPE_REPRESENTATION(#79,#11986);
#146=CONTEXT_DEPENDENT_SHAPE_REPRESENTATION(#80,#11987);
#147=CONTEXT_DEPENDENT_SHAPE_REPRESENTATION(#81,#11988);
#148=CONTEXT_DEPENDENT_SHAPE_REPRESENTATION(#82,#12014);
#149=CONTEXT_DEPENDENT_SHAPE_REPRESENTATION(#83,#12015);
#150=CONTEXT_DEPENDENT_SHAPE_REPRESENTATION(#84,#12016);
#151=CONTEXT_DEPENDENT_SHAPE_REPRESENTATION(#85,#12017);
#152=CONTEXT_DEPENDENT_SHAPE_REPRESENTATION(#86,#12018);
#153=CONTEXT_DEPENDENT_SHAPE_REPRESENTATION(#87,#12019);
#154=CONTEXT_DEPENDENT_SHAPE_REPRESENTATION(#88,#12020);
#155=CONTEXT_DEPENDENT_SHAPE_REPRESENTATION(#89,#12021);
#156=CONTEXT_DEPENDENT_SHAPE_REPRESENTATION(#90,#12022);
#157=CONTEXT_DEPENDENT_SHAPE_REPRESENTATION(#91,#12023);
#158=CONTEXT_DEPENDENT_SHAPE_REPRESENTATION(#92,#12024);
#159=CONTEXT_DEPENDENT_SHAPE_REPRESENTATION(#93,#12025);
#160=CONTEXT_DEPENDENT_SHAPE_REPRESENTATION(#94,#12026);
#161=CONTEXT_DEPENDENT_SHAPE_REPRESENTATION(#95,#12027);
#162=CONTEXT_DEPENDENT_SHAPE_REPRESENTATION(#96,#12028);
#163=CONTEXT_DEPENDENT_SHAPE_REPRESENTATION(#97,#12029);
#164=CONTEXT_DEPENDENT_SHAPE_REPRESENTATION(#98,#12030);
#165=CONTEXT_DEPENDENT_SHAPE_REPRESENTATION(#99,#12031);
#166=CONTEXT_DEPENDENT_SHAPE_REPRESENTATION(#100,#12032);
#167=CONTEXT_DEPENDENT_SHAPE_REPRESENTATION(#101,#12033);
#168=CONTEXT_DEPENDENT_SHAPE_REPRESENTATION(#102,#12034);
#169=CONTEXT_DEPENDENT_SHAPE_REPRESENTATION(#103,#12035);
#170=CONTEXT_DEPENDENT_SHAPE_REPRESENTATION(#104,#12036);
#171=CONTEXT_DEPENDENT_SHAPE_REPRESENTATION(#105,#12037);
#172=CONTEXT_DEPENDENT_SHAPE_REPRESENTATION(#106,#12038);
#173=CONTEXT_DEPENDENT_SHAPE_REPRESENTATION(#107,#12039);
#174=CONTEXT_DEPENDENT_SHAPE_REPRESENTATION(#108,#12040);
#175=CONTEXT_DEPENDENT_SHAPE_REPRESENTATION(#109,#12041);
#176=CONTEXT_DEPENDENT_SHAPE_REPRESENTATION(#110,#12042);
#177=CONTEXT_DEPENDENT_SHAPE_REPRESENTATION(#111,#12043);
#178=CONTEXT_DEPENDENT_SHAPE_REPRESENTATION(#112,#12044);
#179=CONTEXT_DEPENDENT_SHAPE_REPRESENTATION(#113,#12045);
#180=CONTEXT_DEPENDENT_SHAPE_REPRESENTATION(#114,#12046);
#181=CONTEXT_DEPENDENT_SHAPE_REPRESENTATION(#115,#12047);
#182=CONTEXT_DEPENDENT_SHAPE_REPRESENTATION(#116,#12048);
#183=CONTEXT_DEPENDENT_SHAPE_REPRESENTATION(#117,#12049);
#184=CONTEXT_DEPENDENT_SHAPE_REPRESENTATION(#118,#12050);
#185=CONTEXT_DEPENDENT_SHAPE_REPRESENTATION(#119,#12051);
#186=CONTEXT_DEPENDENT_SHAPE_REPRESENTATION(#120,#12052);
#187=CONTEXT_DEPENDENT_SHAPE_REPRESENTATION(#121,#12053);
#188=CONTEXT_DEPENDENT_SHAPE_REPRESENTATION(#122,#12054);
#189=CONTEXT_DEPENDENT_SHAPE_REPRESENTATION(#123,#12055);
#190=CONTEXT_DEPENDENT_SHAPE_REPRESENTATION(#124,#12056);
#191=CONTEXT_DEPENDENT_SHAPE_REPRESENTATION(#125,#12057);
#192=CONTEXT_DEPENDENT_SHAPE_REPRESENTATION(#126,#12058);
#193=CONTEXT_DEPENDENT_SHAPE_REPRESENTATION(#127,#12059);
#194=CONTEXT_DEPENDENT_SHAPE_REPRESENTATION(#128,#12060);
#195=CONTEXT_DEPENDENT_SHAPE_REPRESENTATION(#129,#12061);
#196=CONTEXT_DEPENDENT_SHAPE_REPRESENTATION(#130,#12062);
#197=CONTEXT_DEPENDENT_SHAPE_REPRESENTATION(#131,#12063);
#198=CONTEXT_DEPENDENT_SHAPE_REPRESENTATION(#132,#12064);
#199=CONTEXT_DEPENDENT_SHAPE_REPRESENTATION(#133,#12065);
#200=CONTEXT_DEPENDENT_SHAPE_REPRESENTATION(#134,#12066);
#201=CONTEXT_DEPENDENT_SHAPE_REPRESENTATION(#135,#12067);
#202=CONTEXT_DEPENDENT_SHAPE_REPRESENTATION(#136,#12072);
#203=CONTEXT_DEPENDENT_SHAPE_REPRESENTATION(#137,#12073);
#204=CONTEXT_DEPENDENT_SHAPE_REPRESENTATION(#138,#12074);
#205=CONTEXT_DEPENDENT_SHAPE_REPRESENTATION(#139,#12075);
#206=CONTEXT_DEPENDENT_SHAPE_REPRESENTATION(#140,#12076);
#207=CONTEXT_DEPENDENT_SHAPE_REPRESENTATION(#141,#12077);
#208=CONTEXT_DEPENDENT_SHAPE_REPRESENTATION(#142,#12078);
#209=NEXT_ASSEMBLY_USAGE_OCCURRENCE('Inner ring:1','Inner ring:1',
'Inner ring:1',#12137,#12138,'Inner ring:1');
#210=NEXT_ASSEMBLY_USAGE_OCCURRENCE('Outer ring:1','Outer ring:1',
'Outer ring:1',#12137,#12139,'Outer ring:1');
#211=NEXT_ASSEMBLY_USAGE_OCCURRENCE('Balls:1','Balls:1','Balls:1',#12137,
#12140,'Balls:1');
#212=NEXT_ASSEMBLY_USAGE_OCCURRENCE('Cage:1','Cage:1','Cage:1',#12137,#12141,
'Cage:1');
#213=NEXT_ASSEMBLY_USAGE_OCCURRENCE('Seals 2RS:1','Seals 2RS:1',
'Seals 2RS:1',#12137,#12142,'Seals 2RS:1');
#214=NEXT_ASSEMBLY_USAGE_OCCURRENCE('Base:1','Base:1','Base:1',#12127,#12128,
'Base:1');
#215=NEXT_ASSEMBLY_USAGE_OCCURRENCE('Foot strip:1','Foot strip:1',
'Foot strip:1',#12127,#12129,'Foot strip:1');
#216=NEXT_ASSEMBLY_USAGE_OCCURRENCE('Foot strip (1):1',
'Foot strip (1):1','Foot strip (1):1',#12127,#12130,'Foot strip (1):1');
#217=NEXT_ASSEMBLY_USAGE_OCCURRENCE('Input pedestal:1',
'Input pedestal:1','Input pedestal:1',#12127,#12131,'Input pedestal:1');
#218=NEXT_ASSEMBLY_USAGE_OCCURRENCE('Input outer spacer:1',
'Input outer spacer:1','Input outer spacer:1',#12127,#12132,
'Input outer spacer:1');
#219=NEXT_ASSEMBLY_USAGE_OCCURRENCE('Input cap:1','Input cap:1',
'Input cap:1',#12127,#12133,'Input cap:1');
#220=NEXT_ASSEMBLY_USAGE_OCCURRENCE('Output pedestal:1',
'Output pedestal:1','Output pedestal:1',#12127,#12134,
'Output pedestal:1');
#221=NEXT_ASSEMBLY_USAGE_OCCURRENCE('Output cap:1','Output cap:1',
'Output cap:1',#12127,#12135,'Output cap:1');
#222=NEXT_ASSEMBLY_USAGE_OCCURRENCE('M5x14 Cap Screw:2',
'M5x14 Cap Screw:2','M5x14 Cap Screw:2',#12127,#12136,
'M5x14 Cap Screw:2');
#223=NEXT_ASSEMBLY_USAGE_OCCURRENCE('M5x14 Cap Screw:3',
'M5x14 Cap Screw:3','M5x14 Cap Screw:3',#12127,#12136,
'M5x14 Cap Screw:3');
#224=NEXT_ASSEMBLY_USAGE_OCCURRENCE('M5x14 Cap Screw:4',
'M5x14 Cap Screw:4','M5x14 Cap Screw:4',#12127,#12136,
'M5x14 Cap Screw:4');
#225=NEXT_ASSEMBLY_USAGE_OCCURRENCE('M5x14 Cap Screw:5',
'M5x14 Cap Screw:5','M5x14 Cap Screw:5',#12127,#12136,
'M5x14 Cap Screw:5');
#226=NEXT_ASSEMBLY_USAGE_OCCURRENCE(
'Sealed Ball Bearing - 10 x 30 x 9 mm:2',
'Sealed Ball Bearing - 10 x 30 x 9 mm:2',
'Sealed Ball Bearing - 10 x 30 x 9 mm:2',#12127,#12137,
'Sealed Ball Bearing - 10 x 30 x 9 mm:2');
#227=NEXT_ASSEMBLY_USAGE_OCCURRENCE(
'Sealed Ball Bearing - 10 x 30 x 9 mm:3',
'Sealed Ball Bearing - 10 x 30 x 9 mm:3',
'Sealed Ball Bearing - 10 x 30 x 9 mm:3',#12127,#12137,
'Sealed Ball Bearing - 10 x 30 x 9 mm:3');
#228=NEXT_ASSEMBLY_USAGE_OCCURRENCE('M4x10 Cap Screw:2',
'M4x10 Cap Screw:2','M4x10 Cap Screw:2',#12127,#12167,
'M4x10 Cap Screw:2');
#229=NEXT_ASSEMBLY_USAGE_OCCURRENCE('M4x10 Cap Screw:3',
'M4x10 Cap Screw:3','M4x10 Cap Screw:3',#12127,#12167,
'M4x10 Cap Screw:3');
#230=NEXT_ASSEMBLY_USAGE_OCCURRENCE('M4x10 Cap Screw:4',
'M4x10 Cap Screw:4','M4x10 Cap Screw:4',#12127,#12167,
'M4x10 Cap Screw:4');
#231=NEXT_ASSEMBLY_USAGE_OCCURRENCE('M4x10 Cap Screw:5',
'M4x10 Cap Screw:5','M4x10 Cap Screw:5',#12127,#12167,
'M4x10 Cap Screw:5');
#232=NEXT_ASSEMBLY_USAGE_OCCURRENCE('M5x14 Cap Screw:6',
'M5x14 Cap Screw:6','M5x14 Cap Screw:6',#12127,#12136,
'M5x14 Cap Screw:6');
#233=NEXT_ASSEMBLY_USAGE_OCCURRENCE('M5x14 Cap Screw:7',
'M5x14 Cap Screw:7','M5x14 Cap Screw:7',#12127,#12136,
'M5x14 Cap Screw:7');
#234=NEXT_ASSEMBLY_USAGE_OCCURRENCE('M5x14 Cap Screw:8',
'M5x14 Cap Screw:8','M5x14 Cap Screw:8',#12127,#12136,
'M5x14 Cap Screw:8');
#235=NEXT_ASSEMBLY_USAGE_OCCURRENCE('M5x14 Cap Screw:9',
'M5x14 Cap Screw:9','M5x14 Cap Screw:9',#12127,#12136,
'M5x14 Cap Screw:9');
#236=NEXT_ASSEMBLY_USAGE_OCCURRENCE(
'Sealed Ball Bearing - 10 x 30 x 9 mm:4',
'Sealed Ball Bearing - 10 x 30 x 9 mm:4',
'Sealed Ball Bearing - 10 x 30 x 9 mm:4',#12127,#12137,
'Sealed Ball Bearing - 10 x 30 x 9 mm:4');
#237=NEXT_ASSEMBLY_USAGE_OCCURRENCE('M4x10 Cap Screw:8',
'M4x10 Cap Screw:8','M4x10 Cap Screw:8',#12127,#12167,
'M4x10 Cap Screw:8');
#238=NEXT_ASSEMBLY_USAGE_OCCURRENCE('M4x10 Cap Screw:9',
'M4x10 Cap Screw:9','M4x10 Cap Screw:9',#12127,#12167,
'M4x10 Cap Screw:9');
#239=NEXT_ASSEMBLY_USAGE_OCCURRENCE('M4x10 Cap Screw:10',
'M4x10 Cap Screw:10','M4x10 Cap Screw:10',#12127,#12167,
'M4x10 Cap Screw:10');
#240=NEXT_ASSEMBLY_USAGE_OCCURRENCE('M4x10 Cap Screw:11',
'M4x10 Cap Screw:11','M4x10 Cap Screw:11',#12127,#12167,
'M4x10 Cap Screw:11');
#241=NEXT_ASSEMBLY_USAGE_OCCURRENCE('Input crank and shaft:1',
'Input crank and shaft:1','Input crank and shaft:1',#12143,#12144,
'Input crank and shaft:1');
#242=NEXT_ASSEMBLY_USAGE_OCCURRENCE('Input inner sleeve:1',
'Input inner sleeve:1','Input inner sleeve:1',#12143,#12145,
'Input inner sleeve:1');
#243=NEXT_ASSEMBLY_USAGE_OCCURRENCE('Intermediate inner sleeve:1',
'Intermediate inner sleeve:1','Intermediate inner sleeve:1',#12143,#12146,
'Intermediate inner sleeve:1');
#244=NEXT_ASSEMBLY_USAGE_OCCURRENCE('Shaft collar:1','Shaft collar:1',
'Shaft collar:1',#12143,#12147,'Shaft collar:1');
#245=NEXT_ASSEMBLY_USAGE_OCCURRENCE('Input knob:1','Input knob:1',
'Input knob:1',#12143,#12148,'Input knob:1');
#246=NEXT_ASSEMBLY_USAGE_OCCURRENCE('Knob keeper:1','Knob keeper:1',
'Knob keeper:1',#12143,#12149,'Knob keeper:1');
#247=NEXT_ASSEMBLY_USAGE_OCCURRENCE('Link pin:1','Link pin:1',
'Link pin:1',#12143,#12150,'Link pin:1');
#248=NEXT_ASSEMBLY_USAGE_OCCURRENCE('Rear link spacer:1',
'Rear link spacer:1','Rear link spacer:1',#12143,#12151,
'Rear link spacer:1');
#249=NEXT_ASSEMBLY_USAGE_OCCURRENCE('Front link spacer:1',
'Front link spacer:1','Front link spacer:1',#12143,#12152,
'Front link spacer:1');
#250=NEXT_ASSEMBLY_USAGE_OCCURRENCE('Lower pin keeper:1',
'Lower pin keeper:1','Lower pin keeper:1',#12143,#12153,
'Lower pin keeper:1');
#251=NEXT_ASSEMBLY_USAGE_OCCURRENCE('Upper pin keeper:1',
'Upper pin keeper:1','Upper pin keeper:1',#12143,#12154,
'Upper pin keeper:1');
#252=NEXT_ASSEMBLY_USAGE_OCCURRENCE('M4x4 collar screw:2',
'M4x4 collar screw:2','M4x4 collar screw:2',#12143,#12165,
'M4x4 collar screw:2');
#253=NEXT_ASSEMBLY_USAGE_OCCURRENCE('Socket Set Screw - M4x6:2',
'Socket Set Screw - M4x6:2','Socket Set Screw - M4x6:2',#12143,#12155,
'Socket Set Screw - M4x6:2');
#254=NEXT_ASSEMBLY_USAGE_OCCURRENCE('M4x10 Cap Screw:6',
'M4x10 Cap Screw:6','M4x10 Cap Screw:6',#12143,#12167,
'M4x10 Cap Screw:6');
#255=NEXT_ASSEMBLY_USAGE_OCCURRENCE('Cap Screw - M4x16:2',
'Cap Screw - M4x16:2','Cap Screw - M4x16:2',#12143,#12166,
'Cap Screw - M4x16:2');
#256=NEXT_ASSEMBLY_USAGE_OCCURRENCE('M4x10 Cap Screw:7',
'M4x10 Cap Screw:7','M4x10 Cap Screw:7',#12143,#12167,
'M4x10 Cap Screw:7');
#257=NEXT_ASSEMBLY_USAGE_OCCURRENCE('Output rocker and post:1',
'Output rocker and post:1','Output rocker and post:1',#12156,#12157,
'Output rocker and post:1');
#258=NEXT_ASSEMBLY_USAGE_OCCURRENCE('Output inner sleeve:1',
'Output inner sleeve:1','Output inner sleeve:1',#12156,#12158,
'Output inner sleeve:1');
#259=NEXT_ASSEMBLY_USAGE_OCCURRENCE('Shaft collar (1):1',
'Shaft collar (1):1','Shaft collar (1):1',#12156,#12159,
'Shaft collar (1):1');
#260=NEXT_ASSEMBLY_USAGE_OCCURRENCE('Link pin (1):1','Link pin (1):1',
'Link pin (1):1',#12156,#12160,'Link pin (1):1');
#261=NEXT_ASSEMBLY_USAGE_OCCURRENCE('Rear link spacer (1):1',
'Rear link spacer (1):1','Rear link spacer (1):1',#12156,#12161,
'Rear link spacer (1):1');
#262=NEXT_ASSEMBLY_USAGE_OCCURRENCE('Front link spacer (1):1',
'Front link spacer (1):1','Front link spacer (1):1',#12156,#12162,
'Front link spacer (1):1');
#263=NEXT_ASSEMBLY_USAGE_OCCURRENCE('Lower pin keeper (1):1',
'Lower pin keeper (1):1','Lower pin keeper (1):1',#12156,#12163,
'Lower pin keeper (1):1');
#264=NEXT_ASSEMBLY_USAGE_OCCURRENCE('Upper pin keeper (1):1',
'Upper pin keeper (1):1','Upper pin keeper (1):1',#12156,#12164,
'Upper pin keeper (1):1');
#265=NEXT_ASSEMBLY_USAGE_OCCURRENCE('M4x4 collar screw:3',
'M4x4 collar screw:3','M4x4 collar screw:3',#12156,#12165,
'M4x4 collar screw:3');
#266=NEXT_ASSEMBLY_USAGE_OCCURRENCE('Cap Screw - M4x16:3',
'Cap Screw - M4x16:3','Cap Screw - M4x16:3',#12156,#12166,
'Cap Screw - M4x16:3');
#267=NEXT_ASSEMBLY_USAGE_OCCURRENCE('M4x10 Cap Screw:12',
'M4x10 Cap Screw:12','M4x10 Cap Screw:12',#12156,#12167,
'M4x10 Cap Screw:12');
#268=NEXT_ASSEMBLY_USAGE_OCCURRENCE('Connecting link:1',
'Connecting link:1','Connecting link:1',#12168,#12169,
'Connecting link:1');
#269=NEXT_ASSEMBLY_USAGE_OCCURRENCE('Link bushing:1','Link bushing:1',
'Link bushing:1',#12168,#12170,'Link bushing:1');
#270=NEXT_ASSEMBLY_USAGE_OCCURRENCE('Link bushing (1):1',
'Link bushing (1):1','Link bushing (1):1',#12168,#12171,
'Link bushing (1):1');
#271=NEXT_ASSEMBLY_USAGE_OCCURRENCE('Bearing base:1','Bearing base:1',
'Bearing base:1',#12126,#12127,'Bearing base:1');
#272=NEXT_ASSEMBLY_USAGE_OCCURRENCE('Continuous input crank:1',
'Continuous input crank:1','Continuous input crank:1',#12126,#12143,
'Continuous input crank:1');
#273=NEXT_ASSEMBLY_USAGE_OCCURRENCE('Oscillating output post:1',
'Oscillating output post:1','Oscillating output post:1',#12126,#12156,
'Oscillating output post:1');
#274=NEXT_ASSEMBLY_USAGE_OCCURRENCE('Connecting link (1):1',
'Connecting link (1):1','Connecting link (1):1',#12126,#12168,
'Connecting link (1):1');
#275=SPHERICAL_SURFACE('',#6871,0.23815);
#276=SPHERICAL_SURFACE('',#6873,0.23815);
#277=SPHERICAL_SURFACE('',#6875,0.23815);
#278=SPHERICAL_SURFACE('',#6877,0.23815);
#279=SPHERICAL_SURFACE('',#6879,0.23815);
#280=SPHERICAL_SURFACE('',#6881,0.23815);
#281=SPHERICAL_SURFACE('',#6883,0.23815);
#282=SPHERICAL_SURFACE('',#6885,0.23815);
#283=SPHERICAL_SURFACE('',#6888,0.247676);
#284=SPHERICAL_SURFACE('',#6904,0.247676);
#285=SPHERICAL_SURFACE('',#6909,0.247676);
#286=SPHERICAL_SURFACE('',#6914,0.247676);
#287=SPHERICAL_SURFACE('',#6919,0.247676);
#288=SPHERICAL_SURFACE('',#6924,0.247676);
#289=SPHERICAL_SURFACE('',#6929,0.247676);
#290=SPHERICAL_SURFACE('',#6937,0.247676);
#291=TOROIDAL_SURFACE('',#6831,1.,0.247676);
#292=TOROIDAL_SURFACE('',#6851,1.,0.247676);
#293=CONICAL_SURFACE('',#6818,0.4,0.785398163397448);
#294=CONICAL_SURFACE('',#6822,0.41,0.785398163397448);
#295=CONICAL_SURFACE('',#6826,0.26,0.463647609000806);
#296=CONICAL_SURFACE('',#6842,0.53,0.785398163397448);
#297=CONICAL_SURFACE('',#6849,0.53,0.785398163397448);
#298=CONICAL_SURFACE('',#6862,1.47,0.785398163397449);
#299=CONICAL_SURFACE('',#6866,1.47,0.785398163397449);
#300=CONICAL_SURFACE('',#7117,0.185,0.785398163397449);
#301=CONICAL_SURFACE('',#7121,0.1625,0.785398163397449);
#302=CONICAL_SURFACE('',#7261,0.185,0.785398163397449);
#303=CONICAL_SURFACE('',#7267,0.325,0.785398163397448);
#304=CONICAL_SURFACE('',#7271,0.335,0.785398163397448);
#305=CONICAL_SURFACE('',#7275,0.21,0.463647609000806);
#306=CONICAL_SURFACE('',#7279,0.18,0.785398163397448);
#307=CONICAL_SURFACE('',#7303,0.325,0.785398163397448);
#308=CONICAL_SURFACE('',#7307,0.335,0.785398163397448);
#309=CONICAL_SURFACE('',#7311,0.21,0.463647609000806);
#310=ORIENTED_CLOSED_SHELL('',*,#6075,.F.);
#311=ORIENTED_CLOSED_SHELL('',*,#6112,.F.);
#312=ORIENTED_CLOSED_SHELL('',*,#6113,.F.);
#313=BREP_WITH_VOIDS('Body1',#6076,(#310));
#314=BREP_WITH_VOIDS('Body1',#6111,(#311));
#315=BREP_WITH_VOIDS('Body1',#6114,(#312));
#316=B_SPLINE_CURVE_WITH_KNOTS('',3,(#9676,#9677,#9678,#9679,#9680,#9681,
#9682,#9683,#9684,#9685),.UNSPECIFIED.,.F.,.F.,(4,2,2,2,4),(0.,0.0945941824764479,
0.189188364952896,0.283770357603024,0.378352350253152),.UNSPECIFIED.);
#317=B_SPLINE_CURVE_WITH_KNOTS('',3,(#9686,#9687,#9688,#9689,#9690,#9691,
#9692,#9693,#9694,#9695,#9696,#9697,#9698,#9699,#9700,#9701,#9702,#9703,
#9704,#9705,#9706,#9707,#9708,#9709,#9710,#9711),.UNSPECIFIED.,.F.,.F.,
(4,2,2,2,2,2,2,2,2,2,2,2,4),(0.378352350253152,0.47293434290328,0.567516335553408,
0.662110518029855,0.756704700506303,0.851298882982751,0.945893065459199,
1.04047505810933,1.13505705075946,1.22963904340958,1.32422103605971,1.41881521853616,
1.51340940101261),.UNSPECIFIED.);
#318=B_SPLINE_CURVE_WITH_KNOTS('',3,(#9715,#9716,#9717,#9718,#9719,#9720,
#9721,#9722,#9723,#9724,#9725,#9726,#9727,#9728,#9729,#9730,#9731,#9732,
#9733,#9734,#9735,#9736,#9737,#9738,#9739,#9740),.UNSPECIFIED.,.F.,.F.,
(4,2,2,2,2,2,2,2,2,2,2,2,4),(0.,0.0942186410044058,0.188437282008812,0.282655768798837,
0.376874255588861,0.471092742378886,0.565311229168911,0.659529870173317,
0.753748511177723,0.847967152182129,0.942185793186535,1.03640427997656,
1.13062276676658),.UNSPECIFIED.);
#319=B_SPLINE_CURVE_WITH_KNOTS('',3,(#9741,#9742,#9743,#9744,#9745,#9746,
#9747,#9748,#9749,#9750),.UNSPECIFIED.,.F.,.F.,(4,2,2,2,4),(1.13062276676658,
1.22484125355661,1.31905974034663,1.41327838135104,1.50749702235545),
 .UNSPECIFIED.);
#320=B_SPLINE_CURVE_WITH_KNOTS('',3,(#9944,#9945,#9946,#9947,#9948,#9949,
#9950,#9951,#9952,#9953),.UNSPECIFIED.,.F.,.F.,(4,2,2,2,4),(0.,0.094594182476448,
0.189188364952896,0.283770357603024,0.378352350253152),.UNSPECIFIED.);
#321=B_SPLINE_CURVE_WITH_KNOTS('',3,(#9954,#9955,#9956,#9957,#9958,#9959,
#9960,#9961,#9962,#9963,#9964,#9965,#9966,#9967,#9968,#9969,#9970,#9971,
#9972,#9973,#9974,#9975,#9976,#9977,#9978,#9979),.UNSPECIFIED.,.F.,.F.,
(4,2,2,2,2,2,2,2,2,2,2,2,4),(0.378352350253152,0.47293434290328,0.567516335553408,
0.662110518029856,0.756704700506304,0.851298882982751,0.945893065459199,
1.04047505810933,1.13505705075946,1.22963904340958,1.32422103605971,1.41881521853616,
1.51340940101261),.UNSPECIFIED.);
#322=B_SPLINE_CURVE_WITH_KNOTS('',3,(#9983,#9984,#9985,#9986,#9987,#9988,
#9989,#9990,#9991,#9992,#9993,#9994,#9995,#9996,#9997,#9998,#9999,#10000,
#10001,#10002,#10003,#10004,#10005,#10006,#10007,#10008),.UNSPECIFIED.,
 .F.,.F.,(4,2,2,2,2,2,2,2,2,2,2,2,4),(0.,0.0942186410044058,0.188437282008812,
0.282655768798837,0.376874255588861,0.471092742378886,0.565311229168911,
0.659529870173317,0.753748511177723,0.847967152182129,0.942185793186535,
1.03640427997656,1.13062276676658),.UNSPECIFIED.);
#323=B_SPLINE_CURVE_WITH_KNOTS('',3,(#10009,#10010,#10011,#10012,#10013,
#10014,#10015,#10016,#10017,#10018),.UNSPECIFIED.,.F.,.F.,(4,2,2,2,4),(1.13062276676658,
1.22484125355661,1.31905974034663,1.41327838135104,1.50749702235545),
 .UNSPECIFIED.);
#324=B_SPLINE_CURVE_WITH_KNOTS('',3,(#10274,#10275,#10276,#10277,#10278,
#10279,#10280,#10281,#10282,#10283,#10284,#10285,#10286,#10287,#10288,#10289,
#10290,#10291,#10292,#10293,#10294,#10295),.UNSPECIFIED.,.F.,.F.,(4,2,2,
2,2,2,2,2,2,2,4),(0.0473477652366656,0.126350602536658,0.189525903804987,
0.252701205073317,0.313298422430275,0.373895639787233,0.434492857144191,
0.495090074501149,0.558265375769478,0.621440677037807,0.7004435143378),
 .UNSPECIFIED.);
#325=B_SPLINE_CURVE_WITH_KNOTS('',3,(#10299,#10300,#10301,#10302,#10303,
#10304,#10305,#10306,#10307,#10308,#10309,#10310,#10311,#10312,#10313,#10314,
#10315,#10316,#10317,#10318,#10319,#10320),.UNSPECIFIED.,.F.,.F.,(4,2,2,
2,2,2,2,2,2,2,4),(0.0464897534940957,0.0852567806515119,0.170513561303024,
0.246687263103517,0.308657850341199,0.370628437578881,0.432599024816563,
0.494569612054245,0.570743313854739,0.656000094506251,0.694767121663666),
 .UNSPECIFIED.);
#326=B_SPLINE_CURVE_WITH_KNOTS('',3,(#10326,#10327,#10328,#10329,#10330,
#10331,#10332,#10333,#10334,#10335,#10336,#10337,#10338,#10339,#10340,#10341,
#10342,#10343,#10344,#10345,#10346,#10347),.UNSPECIFIED.,.F.,.F.,(4,2,2,
2,2,2,2,2,2,2,4),(0.0464897534940957,0.0852567806515118,0.170513561303024,
0.246687263103517,0.308657850341199,0.370628437578881,0.432599024816563,
0.494569612054245,0.570743313854738,0.65600009450625,0.694767121663666),
 .UNSPECIFIED.);
#327=B_SPLINE_CURVE_WITH_KNOTS('',3,(#10351,#10352,#10353,#10354,#10355,
#10356,#10357,#10358,#10359,#10360,#10361,#10362,#10363,#10364,#10365,#10366,
#10367,#10368,#10369,#10370,#10371,#10372),.UNSPECIFIED.,.F.,.F.,(4,2,2,
2,2,2,2,2,2,2,4),(0.0464897534940957,0.0852567806515119,0.170513561303024,
0.246687263103517,0.308657850341199,0.370628437578881,0.432599024816563,
0.494569612054245,0.570743313854739,0.656000094506251,0.694767121663666),
 .UNSPECIFIED.);
#328=B_SPLINE_CURVE_WITH_KNOTS('',3,(#10376,#10377,#10378,#10379,#10380,
#10381,#10382,#10383,#10384,#10385,#10386,#10387),.UNSPECIFIED.,.F.,.F.,
(4,2,2,2,2,4),(0.0464897534940957,0.0852567806515119,0.170513561303024,
0.246687263103517,0.308657850341199,0.370628437578881),.UNSPECIFIED.);
#329=B_SPLINE_CURVE_WITH_KNOTS('',3,(#10392,#10393,#10394,#10395,#10396,
#10397,#10398,#10399,#10400,#10401,#10402,#10403),.UNSPECIFIED.,.F.,.F.,
(4,2,2,2,2,4),(0.370628437578881,0.432599024816563,0.494569612054245,0.570743313854738,
0.65600009450625,0.694767121663666),.UNSPECIFIED.);
#330=B_SPLINE_CURVE_WITH_KNOTS('',3,(#10407,#10408,#10409,#10410,#10411,
#10412,#10413,#10414,#10415,#10416,#10417,#10418,#10419,#10420,#10421,#10422,
#10423,#10424,#10425,#10426,#10427,#10428),.UNSPECIFIED.,.F.,.F.,(4,2,2,
2,2,2,2,2,2,2,4),(0.0464897534940957,0.0852567806515121,0.170513561303024,
0.246687263103518,0.308657850341199,0.370628437578881,0.432599024816563,
0.494569612054245,0.570743313854738,0.65600009450625,0.694767121663666),
 .UNSPECIFIED.);
#331=B_SPLINE_CURVE_WITH_KNOTS('',3,(#10432,#10433,#10434,#10435,#10436,
#10437,#10438,#10439,#10440,#10441,#10442,#10443,#10444,#10445,#10446,#10447,
#10448,#10449,#10450,#10451,#10452,#10453),.UNSPECIFIED.,.F.,.F.,(4,2,2,
2,2,2,2,2,2,2,4),(0.0464897534940957,0.0852567806515119,0.170513561303024,
0.246687263103517,0.308657850341199,0.370628437578881,0.432599024816563,
0.494569612054245,0.570743313854738,0.65600009450625,0.694767121663667),
 .UNSPECIFIED.);
#332=B_SPLINE_CURVE_WITH_KNOTS('',3,(#10457,#10458,#10459,#10460,#10461,
#10462,#10463,#10464,#10465,#10466,#10467,#10468,#10469,#10470,#10471,#10472,
#10473,#10474,#10475,#10476,#10477,#10478),.UNSPECIFIED.,.F.,.F.,(4,2,2,
2,2,2,2,2,2,2,4),(0.0464897534940957,0.0852567806515119,0.170513561303024,
0.246687263103517,0.308657850341199,0.370628437578881,0.432599024816563,
0.494569612054245,0.570743313854738,0.65600009450625,0.694767121663666),
 .UNSPECIFIED.);
#333=B_SPLINE_CURVE_WITH_KNOTS('',3,(#10482,#10483,#10484,#10485,#10486,
#10487,#10488,#10489,#10490,#10491,#10492,#10493,#10494,#10495,#10496,#10497,
#10498,#10499,#10500,#10501,#10502,#10503),.UNSPECIFIED.,.F.,.F.,(4,2,2,
2,2,2,2,2,2,2,4),(0.0464897534940957,0.0852567806515119,0.170513561303024,
0.246687263103517,0.308657850341199,0.370628437578881,0.432599024816563,
0.494569612054245,0.570743313854739,0.656000094506251,0.694767121663667),
 .UNSPECIFIED.);
#334=B_SPLINE_CURVE_WITH_KNOTS('',3,(#10511,#10512,#10513,#10514,#10515,
#10516,#10517,#10518,#10519,#10520,#10521,#10522,#10523,#10524,#10525,#10526,
#10527,#10528,#10529,#10530,#10531,#10532),.UNSPECIFIED.,.F.,.F.,(4,2,2,
2,2,2,2,2,2,2,4),(0.0473477652366656,0.126350602536658,0.189525903804987,
0.252701205073316,0.313298422430274,0.373895639787232,0.434492857144191,
0.495090074501149,0.558265375769478,0.621440677037807,0.7004435143378),
 .UNSPECIFIED.);
#335=B_SPLINE_CURVE_WITH_KNOTS('',3,(#10540,#10541,#10542,#10543,#10544,
#10545,#10546,#10547,#10548,#10549,#10550,#10551,#10552,#10553,#10554,#10555,
#10556,#10557,#10558,#10559,#10560,#10561),.UNSPECIFIED.,.F.,.F.,(4,2,2,
2,2,2,2,2,2,2,4),(0.0473477652366656,0.126350602536658,0.189525903804987,
0.252701205073317,0.313298422430275,0.373895639787233,0.434492857144191,
0.495090074501149,0.558265375769478,0.621440677037807,0.7004435143378),
 .UNSPECIFIED.);
#336=B_SPLINE_CURVE_WITH_KNOTS('',3,(#10570,#10571,#10572,#10573,#10574,
#10575,#10576,#10577,#10578,#10579,#10580,#10581),.UNSPECIFIED.,.F.,.F.,
(4,2,2,2,2,4),(0.0473477652366656,0.126350602536658,0.189525903804987,0.252701205073316,
0.313298422430275,0.373895639787233),.UNSPECIFIED.);
#337=B_SPLINE_CURVE_WITH_KNOTS('',3,(#10583,#10584,#10585,#10586,#10587,
#10588,#10589,#10590,#10591,#10592,#10593,#10594),.UNSPECIFIED.,.F.,.F.,
(4,2,2,2,2,4),(0.373895639787233,0.434492857144191,0.495090074501149,0.558265375769478,
0.621440677037807,0.7004435143378),.UNSPECIFIED.);
#338=B_SPLINE_CURVE_WITH_KNOTS('',3,(#10601,#10602,#10603,#10604,#10605,
#10606,#10607,#10608,#10609,#10610,#10611,#10612,#10613,#10614,#10615,#10616,
#10617,#10618,#10619,#10620,#10621,#10622),.UNSPECIFIED.,.F.,.F.,(4,2,2,
2,2,2,2,2,2,2,4),(0.0473477652366656,0.126350602536658,0.189525903804987,
0.252701205073316,0.313298422430275,0.373895639787233,0.434492857144191,
0.495090074501149,0.558265375769478,0.621440677037807,0.7004435143378),
 .UNSPECIFIED.);
#339=B_SPLINE_CURVE_WITH_KNOTS('',3,(#10630,#10631,#10632,#10633,#10634,
#10635,#10636,#10637,#10638,#10639,#10640,#10641,#10642,#10643,#10644,#10645,
#10646,#10647,#10648,#10649,#10650,#10651),.UNSPECIFIED.,.F.,.F.,(4,2,2,
2,2,2,2,2,2,2,4),(0.0473477652366656,0.126350602536658,0.189525903804987,
0.252701205073317,0.313298422430275,0.373895639787233,0.434492857144191,
0.495090074501149,0.558265375769478,0.621440677037807,0.7004435143378),
 .UNSPECIFIED.);
#340=B_SPLINE_CURVE_WITH_KNOTS('',3,(#10659,#10660,#10661,#10662,#10663,
#10664,#10665,#10666,#10667,#10668,#10669,#10670,#10671,#10672,#10673,#10674,
#10675,#10676,#10677,#10678,#10679,#10680),.UNSPECIFIED.,.F.,.F.,(4,2,2,
2,2,2,2,2,2,2,4),(0.0473477652366656,0.126350602536658,0.189525903804987,
0.252701205073316,0.313298422430275,0.373895639787233,0.434492857144191,
0.495090074501149,0.558265375769478,0.621440677037807,0.7004435143378),
 .UNSPECIFIED.);
#341=B_SPLINE_CURVE_WITH_KNOTS('',3,(#10689,#10690,#10691,#10692,#10693,
#10694,#10695,#10696,#10697,#10698,#10699,#10700,#10701,#10702,#10703,#10704,
#10705,#10706,#10707,#10708,#10709,#10710),.UNSPECIFIED.,.F.,.F.,(4,2,2,
2,2,2,2,2,2,2,4),(0.0473477652366656,0.126350602536658,0.189525903804987,
0.252701205073317,0.313298422430275,0.373895639787233,0.434492857144191,
0.495090074501149,0.558265375769478,0.621440677037807,0.7004435143378),
 .UNSPECIFIED.);
#342=B_SPLINE_CURVE_WITH_KNOTS('',3,(#10852,#10853,#10854,#10855,#10856,
#10857,#10858,#10859,#10860,#10861,#10862,#10863,#10864,#10865),
 .UNSPECIFIED.,.F.,.F.,(4,2,2,2,2,2,4),(0.618551524396293,0.626563103102765,
0.689203386094988,0.751843669087211,0.814483952079434,0.877124235071657,
0.88513581377813),.UNSPECIFIED.);
#343=B_SPLINE_CURVE_WITH_KNOTS('',3,(#10869,#10870,#10871,#10872,#10873,
#10874,#10875,#10876),.UNSPECIFIED.,.F.,.F.,(4,2,2,4),(0.250614556362404,
0.313254839354627,0.37589512234685,0.383906701053323),.UNSPECIFIED.);
#344=B_SPLINE_CURVE_WITH_KNOTS('',3,(#10880,#10881,#10882,#10883,#10884,
#10885,#10886,#10887,#10888,#10889,#10890,#10891,#10892,#10893,#10894,#10895,
#10896,#10897,#10898,#10899,#10900,#10901,#10902,#10903,#10904,#10905),
 .UNSPECIFIED.,.F.,.F.,(4,2,2,2,2,2,2,2,2,2,2,2,4),(0.,0.0623062782223143,
0.124612556444629,0.186916384615149,0.249220212785669,0.31152404095619,
0.37382786912671,0.436134147349024,0.498440425571339,0.560746703793653,
0.623052982015967,0.685356810186488,0.747660638357008),.UNSPECIFIED.);
#345=B_SPLINE_CURVE_WITH_KNOTS('',3,(#10906,#10907,#10908,#10909,#10910,
#10911,#10912,#10913,#10914,#10915),.UNSPECIFIED.,.F.,.F.,(4,2,2,2,4),(0.747660638357008,
0.809964466527528,0.872268294698049,0.934574572920363,0.996880851142677),
 .UNSPECIFIED.);
#346=B_SPLINE_CURVE_WITH_KNOTS('',3,(#10916,#10917,#10918,#10919,#10920,
#10921,#10922,#10923),.UNSPECIFIED.,.F.,.F.,(4,2,2,4),(0.117322411671485,
0.125333990377958,0.187974273370181,0.250614556362404),.UNSPECIFIED.);
#347=B_SPLINE_CURVE_WITH_KNOTS('',3,(#10948,#10949,#10950,#10951,#10952,
#10953,#10954,#10955,#10956,#10957),.UNSPECIFIED.,.F.,.F.,(4,2,2,2,4),(0.649292020015383,
0.689320963667327,0.7519713082482,0.814621652829073,0.854650596481017),
 .UNSPECIFIED.);
#348=B_SPLINE_CURVE_WITH_KNOTS('',3,(#10961,#10962,#10963,#10964,#10965,
#10966),.UNSPECIFIED.,.F.,.F.,(4,2,4),(0.2506571027494,0.313307447330273,
0.353336390982217),.UNSPECIFIED.);
#349=B_SPLINE_CURVE_WITH_KNOTS('',3,(#10970,#10971,#10972,#10973,#10974,
#10975,#10976,#10977,#10978,#10979,#10980,#10981,#10982,#10983,#10984,#10985,
#10986,#10987,#10988,#10989,#10990,#10991,#10992,#10993,#10994,#10995),
 .UNSPECIFIED.,.F.,.F.,(4,2,2,2,2,2,2,2,2,2,2,2,4),(0.,0.0622384309821294,
0.124476861964259,0.186714529331343,0.248952196698428,0.311189864065512,
0.373427531432596,0.435665962414726,0.497904393396855,0.560142824378985,
0.622381255361114,0.684618922728198,0.746856590095283),.UNSPECIFIED.);
#350=B_SPLINE_CURVE_WITH_KNOTS('',3,(#10996,#10997,#10998,#10999,#11000,
#11001,#11002,#11003,#11004,#11005),.UNSPECIFIED.,.F.,.F.,(4,2,2,2,4),(0.746856590095283,
0.809094257462367,0.871331924829452,0.933570355811581,0.99580878679371),
 .UNSPECIFIED.);
#351=B_SPLINE_CURVE_WITH_KNOTS('',3,(#11006,#11007,#11008,#11009,#11010,
#11011),.UNSPECIFIED.,.F.,.F.,(4,2,4),(0.147977814516583,0.188006758168527,
0.2506571027494),.UNSPECIFIED.);
#352=B_SPLINE_CURVE_WITH_KNOTS('',3,(#11321,#11322,#11323,#11324,#11325,
#11326,#11327,#11328,#11329,#11330,#11331,#11332,#11333,#11334),
 .UNSPECIFIED.,.F.,.F.,(4,2,2,2,2,2,4),(0.618551524396289,0.626563103102765,
0.689203386094988,0.751843669087211,0.814483952079434,0.877124235071657,
0.885135813778134),.UNSPECIFIED.);
#353=B_SPLINE_CURVE_WITH_KNOTS('',3,(#11338,#11339,#11340,#11341,#11342,
#11343,#11344,#11345),.UNSPECIFIED.,.F.,.F.,(4,2,2,4),(0.250614556362404,
0.313254839354627,0.37589512234685,0.383906701053326),.UNSPECIFIED.);
#354=B_SPLINE_CURVE_WITH_KNOTS('',3,(#11349,#11350,#11351,#11352,#11353,
#11354,#11355,#11356,#11357,#11358,#11359,#11360,#11361,#11362,#11363,#11364,
#11365,#11366,#11367,#11368,#11369,#11370,#11371,#11372,#11373,#11374),
 .UNSPECIFIED.,.F.,.F.,(4,2,2,2,2,2,2,2,2,2,2,2,4),(0.,0.0623062782223143,
0.124612556444629,0.186916384615149,0.249220212785669,0.31152404095619,
0.37382786912671,0.436134147349024,0.498440425571339,0.560746703793653,
0.623052982015967,0.685356810186488,0.747660638357008),.UNSPECIFIED.);
#355=B_SPLINE_CURVE_WITH_KNOTS('',3,(#11375,#11376,#11377,#11378,#11379,
#11380,#11381,#11382,#11383,#11384),.UNSPECIFIED.,.F.,.F.,(4,2,2,2,4),(0.747660638357008,
0.809964466527529,0.872268294698049,0.934574572920363,0.996880851142677),
 .UNSPECIFIED.);
#356=B_SPLINE_CURVE_WITH_KNOTS('',3,(#11385,#11386,#11387,#11388,#11389,
#11390,#11391,#11392),.UNSPECIFIED.,.F.,.F.,(4,2,2,4),(0.117322411671481,
0.125333990377958,0.187974273370181,0.250614556362404),.UNSPECIFIED.);
#357=SHAPE_REPRESENTATION_RELATIONSHIP('SRR','None',#12081,#397);
#358=SHAPE_REPRESENTATION_RELATIONSHIP('SRR','None',#12082,#398);
#359=SHAPE_REPRESENTATION_RELATIONSHIP('SRR','None',#12083,#399);
#360=SHAPE_REPRESENTATION_RELATIONSHIP('SRR','None',#12084,#400);
#361=SHAPE_REPRESENTATION_RELATIONSHIP('SRR','None',#12085,#401);
#362=SHAPE_REPRESENTATION_RELATIONSHIP('SRR','None',#12086,#402);
#363=SHAPE_REPRESENTATION_RELATIONSHIP('SRR','None',#12087,#403);
#364=SHAPE_REPRESENTATION_RELATIONSHIP('SRR','None',#12088,#404);
#365=SHAPE_REPRESENTATION_RELATIONSHIP('SRR','None',#12089,#405);
#366=SHAPE_REPRESENTATION_RELATIONSHIP('SRR','None',#12091,#406);
#367=SHAPE_REPRESENTATION_RELATIONSHIP('SRR','None',#12092,#407);
#368=SHAPE_REPRESENTATION_RELATIONSHIP('SRR','None',#12093,#408);
#369=SHAPE_REPRESENTATION_RELATIONSHIP('SRR','None',#12094,#409);
#370=SHAPE_REPRESENTATION_RELATIONSHIP('SRR','None',#12095,#410);
#371=SHAPE_REPRESENTATION_RELATIONSHIP('SRR','None',#12097,#411);
#372=SHAPE_REPRESENTATION_RELATIONSHIP('SRR','None',#12098,#412);
#373=SHAPE_REPRESENTATION_RELATIONSHIP('SRR','None',#12099,#413);
#374=SHAPE_REPRESENTATION_RELATIONSHIP('SRR','None',#12100,#414);
#375=SHAPE_REPRESENTATION_RELATIONSHIP('SRR','None',#12101,#415);
#376=SHAPE_REPRESENTATION_RELATIONSHIP('SRR','None',#12102,#416);
#377=SHAPE_REPRESENTATION_RELATIONSHIP('SRR','None',#12103,#417);
#378=SHAPE_REPRESENTATION_RELATIONSHIP('SRR','None',#12104,#418);
#379=SHAPE_REPRESENTATION_RELATIONSHIP('SRR','None',#12105,#419);
#380=SHAPE_REPRESENTATION_RELATIONSHIP('SRR','None',#12106,#420);
#381=SHAPE_REPRESENTATION_RELATIONSHIP('SRR','None',#12107,#421);
#382=SHAPE_REPRESENTATION_RELATIONSHIP('SRR','None',#12108,#422);
#383=SHAPE_REPRESENTATION_RELATIONSHIP('SRR','None',#12110,#423);
#384=SHAPE_REPRESENTATION_RELATIONSHIP('SRR','None',#12111,#424);
#385=SHAPE_REPRESENTATION_RELATIONSHIP('SRR','None',#12112,#425);
#386=SHAPE_REPRESENTATION_RELATIONSHIP('SRR','None',#12113,#426);
#387=SHAPE_REPRESENTATION_RELATIONSHIP('SRR','None',#12114,#427);
#388=SHAPE_REPRESENTATION_RELATIONSHIP('SRR','None',#12115,#428);
#389=SHAPE_REPRESENTATION_RELATIONSHIP('SRR','None',#12116,#429);
#390=SHAPE_REPRESENTATION_RELATIONSHIP('SRR','None',#12117,#430);
#391=SHAPE_REPRESENTATION_RELATIONSHIP('SRR','None',#12118,#431);
#392=SHAPE_REPRESENTATION_RELATIONSHIP('SRR','None',#12119,#432);
#393=SHAPE_REPRESENTATION_RELATIONSHIP('SRR','None',#12120,#433);
#394=SHAPE_REPRESENTATION_RELATIONSHIP('SRR','None',#12122,#434);
#395=SHAPE_REPRESENTATION_RELATIONSHIP('SRR','None',#12123,#435);
#396=SHAPE_REPRESENTATION_RELATIONSHIP('SRR','None',#12124,#436);
#397=ADVANCED_BREP_SHAPE_REPRESENTATION('',(#485),#11872);
#398=ADVANCED_BREP_SHAPE_REPRESENTATION('',(#486),#11873);
#399=ADVANCED_BREP_SHAPE_REPRESENTATION('',(#487),#11874);
#400=ADVANCED_BREP_SHAPE_REPRESENTATION('',(#488),#11875);
#401=ADVANCED_BREP_SHAPE_REPRESENTATION('',(#489),#11876);
#402=ADVANCED_BREP_SHAPE_REPRESENTATION('',(#490),#11877);
#403=ADVANCED_BREP_SHAPE_REPRESENTATION('',(#491),#11878);
#404=ADVANCED_BREP_SHAPE_REPRESENTATION('',(#492),#11879);
#405=ADVANCED_BREP_SHAPE_REPRESENTATION('',(#313),#11880);
#406=ADVANCED_BREP_SHAPE_REPRESENTATION('',(#493),#11882);
#407=ADVANCED_BREP_SHAPE_REPRESENTATION('',(#494),#11883);
#408=ADVANCED_BREP_SHAPE_REPRESENTATION('',(#495,#496,#497,#498,#499,#500,
#501,#502),#11884);
#409=ADVANCED_BREP_SHAPE_REPRESENTATION('',(#503),#11885);
#410=ADVANCED_BREP_SHAPE_REPRESENTATION('',(#504,#505),#11886);
#411=ADVANCED_BREP_SHAPE_REPRESENTATION('',(#506),#11888);
#412=ADVANCED_BREP_SHAPE_REPRESENTATION('',(#507),#11889);
#413=ADVANCED_BREP_SHAPE_REPRESENTATION('',(#508),#11890);
#414=ADVANCED_BREP_SHAPE_REPRESENTATION('',(#509),#11891);
#415=ADVANCED_BREP_SHAPE_REPRESENTATION('',(#510),#11892);
#416=ADVANCED_BREP_SHAPE_REPRESENTATION('',(#511),#11893);
#417=ADVANCED_BREP_SHAPE_REPRESENTATION('',(#512),#11894);
#418=ADVANCED_BREP_SHAPE_REPRESENTATION('',(#513),#11895);
#419=ADVANCED_BREP_SHAPE_REPRESENTATION('',(#514),#11896);
#420=ADVANCED_BREP_SHAPE_REPRESENTATION('',(#515),#11897);
#421=ADVANCED_BREP_SHAPE_REPRESENTATION('',(#516),#11898);
#422=ADVANCED_BREP_SHAPE_REPRESENTATION('',(#517),#11899);
#423=ADVANCED_BREP_SHAPE_REPRESENTATION('',(#518),#11901);
#424=ADVANCED_BREP_SHAPE_REPRESENTATION('',(#519),#11902);
#425=ADVANCED_BREP_SHAPE_REPRESENTATION('',(#520),#11903);
#426=ADVANCED_BREP_SHAPE_REPRESENTATION('',(#521),#11904);
#427=ADVANCED_BREP_SHAPE_REPRESENTATION('',(#522),#11905);
#428=ADVANCED_BREP_SHAPE_REPRESENTATION('',(#523),#11906);
#429=ADVANCED_BREP_SHAPE_REPRESENTATION('',(#524),#11907);
#430=ADVANCED_BREP_SHAPE_REPRESENTATION('',(#525),#11908);
#431=ADVANCED_BREP_SHAPE_REPRESENTATION('',(#526),#11909);
#432=ADVANCED_BREP_SHAPE_REPRESENTATION('',(#314),#11910);
#433=ADVANCED_BREP_SHAPE_REPRESENTATION('',(#315),#11911);
#434=ADVANCED_BREP_SHAPE_REPRESENTATION('',(#527),#11913);
#435=ADVANCED_BREP_SHAPE_REPRESENTATION('',(#528),#11914);
#436=ADVANCED_BREP_SHAPE_REPRESENTATION('',(#529),#11915);
#437=STYLED_ITEM('',(#12354),#485);
#438=STYLED_ITEM('',(#12361),#486);
#439=STYLED_ITEM('',(#12361),#487);
#440=STYLED_ITEM('',(#12389),#488);
#441=STYLED_ITEM('',(#12368),#489);
#442=STYLED_ITEM('',(#12368),#490);
#443=STYLED_ITEM('',(#12368),#491);
#444=STYLED_ITEM('',(#12361),#492);
#445=STYLED_ITEM('',(#12382),#313);
#446=STYLED_ITEM('',(#12375),#493);
#447=STYLED_ITEM('',(#12375),#494);
#448=STYLED_ITEM('',(#12375),#495);
#449=STYLED_ITEM('',(#12375),#496);
#450=STYLED_ITEM('',(#12375),#497);
#451=STYLED_ITEM('',(#12375),#498);
#452=STYLED_ITEM('',(#12375),#499);
#453=STYLED_ITEM('',(#12375),#500);
#454=STYLED_ITEM('',(#12375),#501);
#455=STYLED_ITEM('',(#12375),#502);
#456=STYLED_ITEM('',(#12375),#503);
#457=STYLED_ITEM('',(#12375),#504);
#458=STYLED_ITEM('',(#12375),#505);
#459=STYLED_ITEM('',(#12375),#506);
#460=STYLED_ITEM('',(#12361),#507);
#461=STYLED_ITEM('',(#12368),#508);
#462=STYLED_ITEM('',(#12375),#509);
#463=STYLED_ITEM('',(#12361),#510);
#464=STYLED_ITEM('',(#12361),#511);
#465=STYLED_ITEM('',(#12375),#512);
#466=STYLED_ITEM('',(#12389),#513);
#467=STYLED_ITEM('',(#12361),#514);
#468=STYLED_ITEM('',(#12375),#515);
#469=STYLED_ITEM('',(#12375),#516);
#470=STYLED_ITEM('',(#12382),#517);
#471=STYLED_ITEM('',(#12361),#518);
#472=STYLED_ITEM('',(#12368),#519);
#473=STYLED_ITEM('',(#12375),#520);
#474=STYLED_ITEM('',(#12375),#521);
#475=STYLED_ITEM('',(#12389),#522);
#476=STYLED_ITEM('',(#12361),#523);
#477=STYLED_ITEM('',(#12375),#524);
#478=STYLED_ITEM('',(#12375),#525);
#479=STYLED_ITEM('',(#12382),#526);
#480=STYLED_ITEM('',(#12382),#314);
#481=STYLED_ITEM('',(#12382),#315);
#482=STYLED_ITEM('',(#12368),#527);
#483=STYLED_ITEM('',(#12361),#528);
#484=STYLED_ITEM('',(#12361),#529);
#485=MANIFOLD_SOLID_BREP('Body1',#6067);
#486=MANIFOLD_SOLID_BREP('Body1',#6068);
#487=MANIFOLD_SOLID_BREP('Body1',#6069);
#488=MANIFOLD_SOLID_BREP('Body1',#6070);
#489=MANIFOLD_SOLID_BREP('Body1',#6071);
#490=MANIFOLD_SOLID_BREP('Body1',#6072);
#491=MANIFOLD_SOLID_BREP('Body1',#6073);
#492=MANIFOLD_SOLID_BREP('Body1',#6074);
#493=MANIFOLD_SOLID_BREP('Body1',#6077);
#494=MANIFOLD_SOLID_BREP('Body1',#6078);
#495=MANIFOLD_SOLID_BREP('Body1',#6079);
#496=MANIFOLD_SOLID_BREP('Body2',#6080);
#497=MANIFOLD_SOLID_BREP('Body3',#6081);
#498=MANIFOLD_SOLID_BREP('Body4',#6082);
#499=MANIFOLD_SOLID_BREP('Body5',#6083);
#500=MANIFOLD_SOLID_BREP('Body6',#6084);
#501=MANIFOLD_SOLID_BREP('Body7',#6085);
#502=MANIFOLD_SOLID_BREP('Body8',#6086);
#503=MANIFOLD_SOLID_BREP('Continuous crown cage',#6087);
#504=MANIFOLD_SOLID_BREP('Body1',#6088);
#505=MANIFOLD_SOLID_BREP('Body2',#6089);
#506=MANIFOLD_SOLID_BREP('Body1',#6090);
#507=MANIFOLD_SOLID_BREP('Body1',#6091);
#508=MANIFOLD_SOLID_BREP('Body1',#6092);
#509=MANIFOLD_SOLID_BREP('Body1',#6093);
#510=MANIFOLD_SOLID_BREP('Body1',#6094);
#511=MANIFOLD_SOLID_BREP('Body1',#6095);
#512=MANIFOLD_SOLID_BREP('Body1',#6096);
#513=MANIFOLD_SOLID_BREP('Body1',#6097);
#514=MANIFOLD_SOLID_BREP('Body1',#6098);
#515=MANIFOLD_SOLID_BREP('Body1',#6099);
#516=MANIFOLD_SOLID_BREP('Body1',#6100);
#517=MANIFOLD_SOLID_BREP('Body1',#6101);
#518=MANIFOLD_SOLID_BREP('Body1',#6102);
#519=MANIFOLD_SOLID_BREP('Body1',#6103);
#520=MANIFOLD_SOLID_BREP('Body1',#6104);
#521=MANIFOLD_SOLID_BREP('Body1',#6105);
#522=MANIFOLD_SOLID_BREP('Body1',#6106);
#523=MANIFOLD_SOLID_BREP('Body1',#6107);
#524=MANIFOLD_SOLID_BREP('Body1',#6108);
#525=MANIFOLD_SOLID_BREP('Body1',#6109);
#526=MANIFOLD_SOLID_BREP('Body1',#6110);
#527=MANIFOLD_SOLID_BREP('Body1',#6115);
#528=MANIFOLD_SOLID_BREP('Body1',#6116);
#529=MANIFOLD_SOLID_BREP('Body1',#6117);
#530=FACE_BOUND('',#1274,.T.);
#531=FACE_BOUND('',#1275,.T.);
#532=FACE_BOUND('',#1276,.T.);
#533=FACE_BOUND('',#1277,.T.);
#534=FACE_BOUND('',#1278,.T.);
#535=FACE_BOUND('',#1279,.T.);
#536=FACE_BOUND('',#1280,.T.);
#537=FACE_BOUND('',#1281,.T.);
#538=FACE_BOUND('',#1283,.T.);
#539=FACE_BOUND('',#1284,.T.);
#540=FACE_BOUND('',#1285,.T.);
#541=FACE_BOUND('',#1286,.T.);
#542=FACE_BOUND('',#1287,.T.);
#543=FACE_BOUND('',#1288,.T.);
#544=FACE_BOUND('',#1289,.T.);
#545=FACE_BOUND('',#1290,.T.);
#546=FACE_BOUND('',#1313,.T.);
#547=FACE_BOUND('',#1314,.T.);
#548=FACE_BOUND('',#1315,.T.);
#549=FACE_BOUND('',#1316,.T.);
#550=FACE_BOUND('',#1317,.T.);
#551=FACE_BOUND('',#1333,.T.);
#552=FACE_BOUND('',#1335,.T.);
#553=FACE_BOUND('',#1337,.T.);
#554=FACE_BOUND('',#1339,.T.);
#555=FACE_BOUND('',#1340,.T.);
#556=FACE_BOUND('',#1341,.T.);
#557=FACE_BOUND('',#1342,.T.);
#558=FACE_BOUND('',#1343,.T.);
#559=FACE_BOUND('',#1345,.T.);
#560=FACE_BOUND('',#1346,.T.);
#561=FACE_BOUND('',#1347,.T.);
#562=FACE_BOUND('',#1348,.T.);
#563=FACE_BOUND('',#1349,.T.);
#564=FACE_BOUND('',#1353,.T.);
#565=FACE_BOUND('',#1355,.T.);
#566=FACE_BOUND('',#1362,.T.);
#567=FACE_BOUND('',#1366,.T.);
#568=FACE_BOUND('',#1367,.T.);
#569=FACE_BOUND('',#1368,.T.);
#570=FACE_BOUND('',#1369,.T.);
#571=FACE_BOUND('',#1370,.T.);
#572=FACE_BOUND('',#1372,.T.);
#573=FACE_BOUND('',#1373,.T.);
#574=FACE_BOUND('',#1374,.T.);
#575=FACE_BOUND('',#1375,.T.);
#576=FACE_BOUND('',#1376,.T.);
#577=FACE_BOUND('',#1387,.T.);
#578=FACE_BOUND('',#1388,.T.);
#579=FACE_BOUND('',#1389,.T.);
#580=FACE_BOUND('',#1390,.T.);
#581=FACE_BOUND('',#1391,.T.);
#582=FACE_BOUND('',#1407,.T.);
#583=FACE_BOUND('',#1409,.T.);
#584=FACE_BOUND('',#1411,.T.);
#585=FACE_BOUND('',#1413,.T.);
#586=FACE_BOUND('',#1414,.T.);
#587=FACE_BOUND('',#1415,.T.);
#588=FACE_BOUND('',#1416,.T.);
#589=FACE_BOUND('',#1417,.T.);
#590=FACE_BOUND('',#1419,.T.);
#591=FACE_BOUND('',#1420,.T.);
#592=FACE_BOUND('',#1421,.T.);
#593=FACE_BOUND('',#1422,.T.);
#594=FACE_BOUND('',#1423,.T.);
#595=FACE_BOUND('',#1430,.T.);
#596=FACE_BOUND('',#1434,.T.);
#597=FACE_BOUND('',#1435,.T.);
#598=FACE_BOUND('',#1436,.T.);
#599=FACE_BOUND('',#1437,.T.);
#600=FACE_BOUND('',#1438,.T.);
#601=FACE_BOUND('',#1440,.T.);
#602=FACE_BOUND('',#1441,.T.);
#603=FACE_BOUND('',#1442,.T.);
#604=FACE_BOUND('',#1443,.T.);
#605=FACE_BOUND('',#1444,.T.);
#606=FACE_BOUND('',#1459,.T.);
#607=FACE_BOUND('',#1467,.T.);
#608=FACE_BOUND('',#1470,.T.);
#609=FACE_BOUND('',#1475,.T.);
#610=FACE_BOUND('',#1480,.T.);
#611=FACE_BOUND('',#1508,.T.);
#612=FACE_BOUND('',#1511,.T.);
#613=FACE_BOUND('',#1514,.T.);
#614=FACE_BOUND('',#1517,.T.);
#615=FACE_BOUND('',#1520,.T.);
#616=FACE_BOUND('',#1528,.T.);
#617=FACE_BOUND('',#1529,.T.);
#618=FACE_BOUND('',#1533,.T.);
#619=FACE_BOUND('',#1534,.T.);
#620=FACE_BOUND('',#1536,.T.);
#621=FACE_BOUND('',#1541,.T.);
#622=FACE_BOUND('',#1546,.T.);
#623=FACE_BOUND('',#1548,.T.);
#624=FACE_BOUND('',#1552,.T.);
#625=FACE_BOUND('',#1554,.T.);
#626=FACE_BOUND('',#1559,.T.);
#627=FACE_BOUND('',#1561,.T.);
#628=FACE_BOUND('',#1563,.T.);
#629=FACE_BOUND('',#1565,.T.);
#630=FACE_BOUND('',#1570,.T.);
#631=FACE_BOUND('',#1572,.T.);
#632=FACE_BOUND('',#1574,.T.);
#633=FACE_BOUND('',#1576,.T.);
#634=FACE_BOUND('',#1580,.T.);
#635=FACE_BOUND('',#1582,.T.);
#636=FACE_BOUND('',#1588,.T.);
#637=FACE_BOUND('',#1590,.T.);
#638=FACE_BOUND('',#1595,.T.);
#639=FACE_BOUND('',#1597,.T.);
#640=FACE_BOUND('',#1601,.T.);
#641=FACE_BOUND('',#1603,.T.);
#642=FACE_BOUND('',#1607,.T.);
#643=FACE_BOUND('',#1609,.T.);
#644=FACE_BOUND('',#1613,.T.);
#645=FACE_BOUND('',#1615,.T.);
#646=FACE_BOUND('',#1619,.T.);
#647=FACE_BOUND('',#1621,.T.);
#648=FACE_BOUND('',#1630,.T.);
#649=FACE_BOUND('',#1640,.T.);
#650=FACE_BOUND('',#1641,.T.);
#651=FACE_BOUND('',#1642,.T.);
#652=FACE_BOUND('',#1643,.T.);
#653=FACE_BOUND('',#1644,.T.);
#654=FACE_BOUND('',#1650,.T.);
#655=FACE_BOUND('',#1651,.T.);
#656=FACE_BOUND('',#1652,.T.);
#657=FACE_BOUND('',#1653,.T.);
#658=FACE_BOUND('',#1659,.T.);
#659=FACE_BOUND('',#1660,.T.);
#660=FACE_BOUND('',#1664,.T.);
#661=FACE_BOUND('',#1665,.T.);
#662=FACE_BOUND('',#1667,.T.);
#663=FACE_BOUND('',#1674,.T.);
#664=FACE_BOUND('',#1676,.T.);
#665=FACE_BOUND('',#1681,.T.);
#666=FACE_BOUND('',#1683,.T.);
#667=FACE_BOUND('',#1685,.T.);
#668=FACE_BOUND('',#1687,.T.);
#669=FACE_BOUND('',#1693,.T.);
#670=FACE_BOUND('',#1695,.T.);
#671=FACE_BOUND('',#1700,.T.);
#672=FACE_BOUND('',#1702,.T.);
#673=FACE_BOUND('',#1706,.T.);
#674=FACE_BOUND('',#1708,.T.);
#675=FACE_BOUND('',#1712,.T.);
#676=FACE_BOUND('',#1714,.T.);
#677=FACE_BOUND('',#1718,.T.);
#678=FACE_BOUND('',#1720,.T.);
#679=FACE_BOUND('',#1724,.T.);
#680=FACE_BOUND('',#1726,.T.);
#681=FACE_BOUND('',#1736,.T.);
#682=FACE_BOUND('',#1744,.T.);
#683=FACE_BOUND('',#1771,.T.);
#684=FACE_BOUND('',#1779,.T.);
#685=FACE_BOUND('',#1780,.T.);
#686=FACE_BOUND('',#1784,.T.);
#687=FACE_BOUND('',#1785,.T.);
#688=FACE_BOUND('',#1789,.T.);
#689=FACE_BOUND('',#1791,.T.);
#690=FACE_BOUND('',#1795,.T.);
#691=FACE_BOUND('',#1797,.T.);
#692=PLANE('',#6586);
#693=PLANE('',#6587);
#694=PLANE('',#6588);
#695=PLANE('',#6589);
#696=PLANE('',#6590);
#697=PLANE('',#6591);
#698=PLANE('',#6593);
#699=PLANE('',#6594);
#700=PLANE('',#6595);
#701=PLANE('',#6596);
#702=PLANE('',#6597);
#703=PLANE('',#6598);
#704=PLANE('',#6600);
#705=PLANE('',#6601);
#706=PLANE('',#6602);
#707=PLANE('',#6603);
#708=PLANE('',#6604);
#709=PLANE('',#6605);
#710=PLANE('',#6607);
#711=PLANE('',#6615);
#712=PLANE('',#6620);
#713=PLANE('',#6625);
#714=PLANE('',#6634);
#715=PLANE('',#6643);
#716=PLANE('',#6647);
#717=PLANE('',#6651);
#718=PLANE('',#6655);
#719=PLANE('',#6668);
#720=PLANE('',#6674);
#721=PLANE('',#6675);
#722=PLANE('',#6683);
#723=PLANE('',#6684);
#724=PLANE('',#6701);
#725=PLANE('',#6708);
#726=PLANE('',#6709);
#727=PLANE('',#6711);
#728=PLANE('',#6719);
#729=PLANE('',#6724);
#730=PLANE('',#6729);
#731=PLANE('',#6738);
#732=PLANE('',#6747);
#733=PLANE('',#6751);
#734=PLANE('',#6755);
#735=PLANE('',#6759);
#736=PLANE('',#6772);
#737=PLANE('',#6778);
#738=PLANE('',#6779);
#739=PLANE('',#6796);
#740=PLANE('',#6803);
#741=PLANE('',#6804);
#742=PLANE('',#6806);
#743=PLANE('',#6807);
#744=PLANE('',#6808);
#745=PLANE('',#6809);
#746=PLANE('',#6810);
#747=PLANE('',#6811);
#748=PLANE('',#6812);
#749=PLANE('',#6813);
#750=PLANE('',#6814);
#751=PLANE('',#6816);
#752=PLANE('',#6824);
#753=PLANE('',#6844);
#754=PLANE('',#6847);
#755=PLANE('',#6859);
#756=PLANE('',#6868);
#757=PLANE('',#6901);
#758=PLANE('',#6906);
#759=PLANE('',#6911);
#760=PLANE('',#6916);
#761=PLANE('',#6921);
#762=PLANE('',#6926);
#763=PLANE('',#6935);
#764=PLANE('',#6939);
#765=PLANE('',#6940);
#766=PLANE('',#6942);
#767=PLANE('',#6947);
#768=PLANE('',#6950);
#769=PLANE('',#6955);
#770=PLANE('',#6968);
#771=PLANE('',#6975);
#772=PLANE('',#6976);
#773=PLANE('',#6979);
#774=PLANE('',#6982);
#775=PLANE('',#6984);
#776=PLANE('',#6992);
#777=PLANE('',#6993);
#778=PLANE('',#7001);
#779=PLANE('',#7002);
#780=PLANE('',#7010);
#781=PLANE('',#7011);
#782=PLANE('',#7013);
#783=PLANE('',#7017);
#784=PLANE('',#7024);
#785=PLANE('',#7025);
#786=PLANE('',#7027);
#787=PLANE('',#7031);
#788=PLANE('',#7038);
#789=PLANE('',#7039);
#790=PLANE('',#7047);
#791=PLANE('',#7048);
#792=PLANE('',#7053);
#793=PLANE('',#7057);
#794=PLANE('',#7058);
#795=PLANE('',#7061);
#796=PLANE('',#7069);
#797=PLANE('',#7070);
#798=PLANE('',#7078);
#799=PLANE('',#7079);
#800=PLANE('',#7087);
#801=PLANE('',#7088);
#802=PLANE('',#7096);
#803=PLANE('',#7097);
#804=PLANE('',#7105);
#805=PLANE('',#7106);
#806=PLANE('',#7108);
#807=PLANE('',#7109);
#808=PLANE('',#7110);
#809=PLANE('',#7111);
#810=PLANE('',#7112);
#811=PLANE('',#7113);
#812=PLANE('',#7114);
#813=PLANE('',#7115);
#814=PLANE('',#7123);
#815=PLANE('',#7138);
#816=PLANE('',#7140);
#817=PLANE('',#7141);
#818=PLANE('',#7142);
#819=PLANE('',#7143);
#820=PLANE('',#7144);
#821=PLANE('',#7153);
#822=PLANE('',#7154);
#823=PLANE('',#7156);
#824=PLANE('',#7159);
#825=PLANE('',#7161);
#826=PLANE('',#7167);
#827=PLANE('',#7175);
#828=PLANE('',#7176);
#829=PLANE('',#7178);
#830=PLANE('',#7182);
#831=PLANE('',#7189);
#832=PLANE('',#7190);
#833=PLANE('',#7195);
#834=PLANE('',#7199);
#835=PLANE('',#7200);
#836=PLANE('',#7203);
#837=PLANE('',#7211);
#838=PLANE('',#7212);
#839=PLANE('',#7220);
#840=PLANE('',#7221);
#841=PLANE('',#7229);
#842=PLANE('',#7230);
#843=PLANE('',#7238);
#844=PLANE('',#7239);
#845=PLANE('',#7247);
#846=PLANE('',#7248);
#847=PLANE('',#7250);
#848=PLANE('',#7252);
#849=PLANE('',#7253);
#850=PLANE('',#7254);
#851=PLANE('',#7255);
#852=PLANE('',#7256);
#853=PLANE('',#7257);
#854=PLANE('',#7258);
#855=PLANE('',#7259);
#856=PLANE('',#7265);
#857=PLANE('',#7273);
#858=PLANE('',#7281);
#859=PLANE('',#7282);
#860=PLANE('',#7283);
#861=PLANE('',#7284);
#862=PLANE('',#7285);
#863=PLANE('',#7286);
#864=PLANE('',#7287);
#865=PLANE('',#7288);
#866=PLANE('',#7289);
#867=PLANE('',#7291);
#868=PLANE('',#7292);
#869=PLANE('',#7293);
#870=PLANE('',#7294);
#871=PLANE('',#7295);
#872=PLANE('',#7296);
#873=PLANE('',#7297);
#874=PLANE('',#7298);
#875=PLANE('',#7299);
#876=PLANE('',#7301);
#877=PLANE('',#7309);
#878=PLANE('',#7379);
#879=PLANE('',#7380);
#880=PLANE('',#7382);
#881=PLANE('',#7385);
#882=PLANE('',#7393);
#883=PLANE('',#7394);
#884=PLANE('',#7402);
#885=PLANE('',#7403);
#886=FACE_OUTER_BOUND('',#1261,.T.);
#887=FACE_OUTER_BOUND('',#1262,.T.);
#888=FACE_OUTER_BOUND('',#1263,.T.);
#889=FACE_OUTER_BOUND('',#1264,.T.);
#890=FACE_OUTER_BOUND('',#1265,.T.);
#891=FACE_OUTER_BOUND('',#1266,.T.);
#892=FACE_OUTER_BOUND('',#1267,.T.);
#893=FACE_OUTER_BOUND('',#1268,.T.);
#894=FACE_OUTER_BOUND('',#1269,.T.);
#895=FACE_OUTER_BOUND('',#1270,.T.);
#896=FACE_OUTER_BOUND('',#1271,.T.);
#897=FACE_OUTER_BOUND('',#1272,.T.);
#898=FACE_OUTER_BOUND('',#1273,.T.);
#899=FACE_OUTER_BOUND('',#1282,.T.);
#900=FACE_OUTER_BOUND('',#1291,.T.);
#901=FACE_OUTER_BOUND('',#1292,.T.);
#902=FACE_OUTER_BOUND('',#1293,.T.);
#903=FACE_OUTER_BOUND('',#1294,.T.);
#904=FACE_OUTER_BOUND('',#1295,.T.);
#905=FACE_OUTER_BOUND('',#1296,.T.);
#906=FACE_OUTER_BOUND('',#1297,.T.);
#907=FACE_OUTER_BOUND('',#1298,.T.);
#908=FACE_OUTER_BOUND('',#1299,.T.);
#909=FACE_OUTER_BOUND('',#1300,.T.);
#910=FACE_OUTER_BOUND('',#1301,.T.);
#911=FACE_OUTER_BOUND('',#1302,.T.);
#912=FACE_OUTER_BOUND('',#1303,.T.);
#913=FACE_OUTER_BOUND('',#1304,.T.);
#914=FACE_OUTER_BOUND('',#1305,.T.);
#915=FACE_OUTER_BOUND('',#1306,.T.);
#916=FACE_OUTER_BOUND('',#1307,.T.);
#917=FACE_OUTER_BOUND('',#1308,.T.);
#918=FACE_OUTER_BOUND('',#1309,.T.);
#919=FACE_OUTER_BOUND('',#1310,.T.);
#920=FACE_OUTER_BOUND('',#1311,.T.);
#921=FACE_OUTER_BOUND('',#1312,.T.);
#922=FACE_OUTER_BOUND('',#1318,.T.);
#923=FACE_OUTER_BOUND('',#1319,.T.);
#924=FACE_OUTER_BOUND('',#1320,.T.);
#925=FACE_OUTER_BOUND('',#1321,.T.);
#926=FACE_OUTER_BOUND('',#1322,.T.);
#927=FACE_OUTER_BOUND('',#1323,.T.);
#928=FACE_OUTER_BOUND('',#1324,.T.);
#929=FACE_OUTER_BOUND('',#1325,.T.);
#930=FACE_OUTER_BOUND('',#1326,.T.);
#931=FACE_OUTER_BOUND('',#1327,.T.);
#932=FACE_OUTER_BOUND('',#1328,.T.);
#933=FACE_OUTER_BOUND('',#1329,.T.);
#934=FACE_OUTER_BOUND('',#1330,.T.);
#935=FACE_OUTER_BOUND('',#1331,.T.);
#936=FACE_OUTER_BOUND('',#1332,.T.);
#937=FACE_OUTER_BOUND('',#1334,.T.);
#938=FACE_OUTER_BOUND('',#1336,.T.);
#939=FACE_OUTER_BOUND('',#1338,.T.);
#940=FACE_OUTER_BOUND('',#1344,.T.);
#941=FACE_OUTER_BOUND('',#1350,.T.);
#942=FACE_OUTER_BOUND('',#1351,.T.);
#943=FACE_OUTER_BOUND('',#1352,.T.);
#944=FACE_OUTER_BOUND('',#1354,.T.);
#945=FACE_OUTER_BOUND('',#1356,.T.);
#946=FACE_OUTER_BOUND('',#1357,.T.);
#947=FACE_OUTER_BOUND('',#1358,.T.);
#948=FACE_OUTER_BOUND('',#1359,.T.);
#949=FACE_OUTER_BOUND('',#1360,.T.);
#950=FACE_OUTER_BOUND('',#1361,.T.);
#951=FACE_OUTER_BOUND('',#1363,.T.);
#952=FACE_OUTER_BOUND('',#1364,.T.);
#953=FACE_OUTER_BOUND('',#1365,.T.);
#954=FACE_OUTER_BOUND('',#1371,.T.);
#955=FACE_OUTER_BOUND('',#1377,.T.);
#956=FACE_OUTER_BOUND('',#1378,.T.);
#957=FACE_OUTER_BOUND('',#1379,.T.);
#958=FACE_OUTER_BOUND('',#1380,.T.);
#959=FACE_OUTER_BOUND('',#1381,.T.);
#960=FACE_OUTER_BOUND('',#1382,.T.);
#961=FACE_OUTER_BOUND('',#1383,.T.);
#962=FACE_OUTER_BOUND('',#1384,.T.);
#963=FACE_OUTER_BOUND('',#1385,.T.);
#964=FACE_OUTER_BOUND('',#1386,.T.);
#965=FACE_OUTER_BOUND('',#1392,.T.);
#966=FACE_OUTER_BOUND('',#1393,.T.);
#967=FACE_OUTER_BOUND('',#1394,.T.);
#968=FACE_OUTER_BOUND('',#1395,.T.);
#969=FACE_OUTER_BOUND('',#1396,.T.);
#970=FACE_OUTER_BOUND('',#1397,.T.);
#971=FACE_OUTER_BOUND('',#1398,.T.);
#972=FACE_OUTER_BOUND('',#1399,.T.);
#973=FACE_OUTER_BOUND('',#1400,.T.);
#974=FACE_OUTER_BOUND('',#1401,.T.);
#975=FACE_OUTER_BOUND('',#1402,.T.);
#976=FACE_OUTER_BOUND('',#1403,.T.);
#977=FACE_OUTER_BOUND('',#1404,.T.);
#978=FACE_OUTER_BOUND('',#1405,.T.);
#979=FACE_OUTER_BOUND('',#1406,.T.);
#980=FACE_OUTER_BOUND('',#1408,.T.);
#981=FACE_OUTER_BOUND('',#1410,.T.);
#982=FACE_OUTER_BOUND('',#1412,.T.);
#983=FACE_OUTER_BOUND('',#1418,.T.);
#984=FACE_OUTER_BOUND('',#1424,.T.);
#985=FACE_OUTER_BOUND('',#1425,.T.);
#986=FACE_OUTER_BOUND('',#1426,.T.);
#987=FACE_OUTER_BOUND('',#1427,.T.);
#988=FACE_OUTER_BOUND('',#1428,.T.);
#989=FACE_OUTER_BOUND('',#1429,.T.);
#990=FACE_OUTER_BOUND('',#1431,.T.);
#991=FACE_OUTER_BOUND('',#1432,.T.);
#992=FACE_OUTER_BOUND('',#1433,.T.);
#993=FACE_OUTER_BOUND('',#1439,.T.);
#994=FACE_OUTER_BOUND('',#1445,.T.);
#995=FACE_OUTER_BOUND('',#1446,.T.);
#996=FACE_OUTER_BOUND('',#1447,.T.);
#997=FACE_OUTER_BOUND('',#1448,.T.);
#998=FACE_OUTER_BOUND('',#1449,.T.);
#999=FACE_OUTER_BOUND('',#1450,.T.);
#1000=FACE_OUTER_BOUND('',#1451,.T.);
#1001=FACE_OUTER_BOUND('',#1452,.T.);
#1002=FACE_OUTER_BOUND('',#1453,.T.);
#1003=FACE_OUTER_BOUND('',#1454,.T.);
#1004=FACE_OUTER_BOUND('',#1455,.T.);
#1005=FACE_OUTER_BOUND('',#1456,.T.);
#1006=FACE_OUTER_BOUND('',#1457,.T.);
#1007=FACE_OUTER_BOUND('',#1458,.T.);
#1008=FACE_OUTER_BOUND('',#1460,.T.);
#1009=FACE_OUTER_BOUND('',#1461,.T.);
#1010=FACE_OUTER_BOUND('',#1462,.T.);
#1011=FACE_OUTER_BOUND('',#1463,.T.);
#1012=FACE_OUTER_BOUND('',#1464,.T.);
#1013=FACE_OUTER_BOUND('',#1465,.T.);
#1014=FACE_OUTER_BOUND('',#1466,.T.);
#1015=FACE_OUTER_BOUND('',#1468,.T.);
#1016=FACE_OUTER_BOUND('',#1469,.T.);
#1017=FACE_OUTER_BOUND('',#1471,.T.);
#1018=FACE_OUTER_BOUND('',#1472,.T.);
#1019=FACE_OUTER_BOUND('',#1473,.T.);
#1020=FACE_OUTER_BOUND('',#1474,.T.);
#1021=FACE_OUTER_BOUND('',#1476,.T.);
#1022=FACE_OUTER_BOUND('',#1477,.T.);
#1023=FACE_OUTER_BOUND('',#1478,.T.);
#1024=FACE_OUTER_BOUND('',#1479,.T.);
#1025=FACE_OUTER_BOUND('',#1481,.T.);
#1026=FACE_OUTER_BOUND('',#1482,.T.);
#1027=FACE_OUTER_BOUND('',#1483,.T.);
#1028=FACE_OUTER_BOUND('',#1484,.T.);
#1029=FACE_OUTER_BOUND('',#1485,.T.);
#1030=FACE_OUTER_BOUND('',#1486,.T.);
#1031=FACE_OUTER_BOUND('',#1487,.T.);
#1032=FACE_OUTER_BOUND('',#1488,.T.);
#1033=FACE_OUTER_BOUND('',#1489,.T.);
#1034=FACE_OUTER_BOUND('',#1490,.T.);
#1035=FACE_OUTER_BOUND('',#1491,.T.);
#1036=FACE_OUTER_BOUND('',#1492,.T.);
#1037=FACE_OUTER_BOUND('',#1493,.T.);
#1038=FACE_OUTER_BOUND('',#1494,.T.);
#1039=FACE_OUTER_BOUND('',#1495,.T.);
#1040=FACE_OUTER_BOUND('',#1496,.T.);
#1041=FACE_OUTER_BOUND('',#1497,.T.);
#1042=FACE_OUTER_BOUND('',#1498,.T.);
#1043=FACE_OUTER_BOUND('',#1499,.T.);
#1044=FACE_OUTER_BOUND('',#1500,.T.);
#1045=FACE_OUTER_BOUND('',#1501,.T.);
#1046=FACE_OUTER_BOUND('',#1502,.T.);
#1047=FACE_OUTER_BOUND('',#1503,.T.);
#1048=FACE_OUTER_BOUND('',#1504,.T.);
#1049=FACE_OUTER_BOUND('',#1505,.T.);
#1050=FACE_OUTER_BOUND('',#1506,.T.);
#1051=FACE_OUTER_BOUND('',#1507,.T.);
#1052=FACE_OUTER_BOUND('',#1509,.T.);
#1053=FACE_OUTER_BOUND('',#1510,.T.);
#1054=FACE_OUTER_BOUND('',#1512,.T.);
#1055=FACE_OUTER_BOUND('',#1513,.T.);
#1056=FACE_OUTER_BOUND('',#1515,.T.);
#1057=FACE_OUTER_BOUND('',#1516,.T.);
#1058=FACE_OUTER_BOUND('',#1518,.T.);
#1059=FACE_OUTER_BOUND('',#1519,.T.);
#1060=FACE_OUTER_BOUND('',#1521,.T.);
#1061=FACE_OUTER_BOUND('',#1522,.T.);
#1062=FACE_OUTER_BOUND('',#1523,.T.);
#1063=FACE_OUTER_BOUND('',#1524,.T.);
#1064=FACE_OUTER_BOUND('',#1525,.T.);
#1065=FACE_OUTER_BOUND('',#1526,.T.);
#1066=FACE_OUTER_BOUND('',#1527,.T.);
#1067=FACE_OUTER_BOUND('',#1530,.T.);
#1068=FACE_OUTER_BOUND('',#1531,.T.);
#1069=FACE_OUTER_BOUND('',#1532,.T.);
#1070=FACE_OUTER_BOUND('',#1535,.T.);
#1071=FACE_OUTER_BOUND('',#1537,.T.);
#1072=FACE_OUTER_BOUND('',#1538,.T.);
#1073=FACE_OUTER_BOUND('',#1539,.T.);
#1074=FACE_OUTER_BOUND('',#1540,.T.);
#1075=FACE_OUTER_BOUND('',#1542,.T.);
#1076=FACE_OUTER_BOUND('',#1543,.T.);
#1077=FACE_OUTER_BOUND('',#1544,.T.);
#1078=FACE_OUTER_BOUND('',#1545,.T.);
#1079=FACE_OUTER_BOUND('',#1547,.T.);
#1080=FACE_OUTER_BOUND('',#1549,.T.);
#1081=FACE_OUTER_BOUND('',#1550,.T.);
#1082=FACE_OUTER_BOUND('',#1551,.T.);
#1083=FACE_OUTER_BOUND('',#1553,.T.);
#1084=FACE_OUTER_BOUND('',#1555,.T.);
#1085=FACE_OUTER_BOUND('',#1556,.T.);
#1086=FACE_OUTER_BOUND('',#1557,.T.);
#1087=FACE_OUTER_BOUND('',#1558,.T.);
#1088=FACE_OUTER_BOUND('',#1560,.T.);
#1089=FACE_OUTER_BOUND('',#1562,.T.);
#1090=FACE_OUTER_BOUND('',#1564,.T.);
#1091=FACE_OUTER_BOUND('',#1566,.T.);
#1092=FACE_OUTER_BOUND('',#1567,.T.);
#1093=FACE_OUTER_BOUND('',#1568,.T.);
#1094=FACE_OUTER_BOUND('',#1569,.T.);
#1095=FACE_OUTER_BOUND('',#1571,.T.);
#1096=FACE_OUTER_BOUND('',#1573,.T.);
#1097=FACE_OUTER_BOUND('',#1575,.T.);
#1098=FACE_OUTER_BOUND('',#1577,.T.);
#1099=FACE_OUTER_BOUND('',#1578,.T.);
#1100=FACE_OUTER_BOUND('',#1579,.T.);
#1101=FACE_OUTER_BOUND('',#1581,.T.);
#1102=FACE_OUTER_BOUND('',#1583,.T.);
#1103=FACE_OUTER_BOUND('',#1584,.T.);
#1104=FACE_OUTER_BOUND('',#1585,.T.);
#1105=FACE_OUTER_BOUND('',#1586,.T.);
#1106=FACE_OUTER_BOUND('',#1587,.T.);
#1107=FACE_OUTER_BOUND('',#1589,.T.);
#1108=FACE_OUTER_BOUND('',#1591,.T.);
#1109=FACE_OUTER_BOUND('',#1592,.T.);
#1110=FACE_OUTER_BOUND('',#1593,.T.);
#1111=FACE_OUTER_BOUND('',#1594,.T.);
#1112=FACE_OUTER_BOUND('',#1596,.T.);
#1113=FACE_OUTER_BOUND('',#1598,.T.);
#1114=FACE_OUTER_BOUND('',#1599,.T.);
#1115=FACE_OUTER_BOUND('',#1600,.T.);
#1116=FACE_OUTER_BOUND('',#1602,.T.);
#1117=FACE_OUTER_BOUND('',#1604,.T.);
#1118=FACE_OUTER_BOUND('',#1605,.T.);
#1119=FACE_OUTER_BOUND('',#1606,.T.);
#1120=FACE_OUTER_BOUND('',#1608,.T.);
#1121=FACE_OUTER_BOUND('',#1610,.T.);
#1122=FACE_OUTER_BOUND('',#1611,.T.);
#1123=FACE_OUTER_BOUND('',#1612,.T.);
#1124=FACE_OUTER_BOUND('',#1614,.T.);
#1125=FACE_OUTER_BOUND('',#1616,.T.);
#1126=FACE_OUTER_BOUND('',#1617,.T.);
#1127=FACE_OUTER_BOUND('',#1618,.T.);
#1128=FACE_OUTER_BOUND('',#1620,.T.);
#1129=FACE_OUTER_BOUND('',#1622,.T.);
#1130=FACE_OUTER_BOUND('',#1623,.T.);
#1131=FACE_OUTER_BOUND('',#1624,.T.);
#1132=FACE_OUTER_BOUND('',#1625,.T.);
#1133=FACE_OUTER_BOUND('',#1626,.T.);
#1134=FACE_OUTER_BOUND('',#1627,.T.);
#1135=FACE_OUTER_BOUND('',#1628,.T.);
#1136=FACE_OUTER_BOUND('',#1629,.T.);
#1137=FACE_OUTER_BOUND('',#1631,.T.);
#1138=FACE_OUTER_BOUND('',#1632,.T.);
#1139=FACE_OUTER_BOUND('',#1633,.T.);
#1140=FACE_OUTER_BOUND('',#1634,.T.);
#1141=FACE_OUTER_BOUND('',#1635,.T.);
#1142=FACE_OUTER_BOUND('',#1636,.T.);
#1143=FACE_OUTER_BOUND('',#1637,.T.);
#1144=FACE_OUTER_BOUND('',#1638,.T.);
#1145=FACE_OUTER_BOUND('',#1639,.T.);
#1146=FACE_OUTER_BOUND('',#1645,.T.);
#1147=FACE_OUTER_BOUND('',#1646,.T.);
#1148=FACE_OUTER_BOUND('',#1647,.T.);
#1149=FACE_OUTER_BOUND('',#1648,.T.);
#1150=FACE_OUTER_BOUND('',#1649,.T.);
#1151=FACE_OUTER_BOUND('',#1654,.T.);
#1152=FACE_OUTER_BOUND('',#1655,.T.);
#1153=FACE_OUTER_BOUND('',#1656,.T.);
#1154=FACE_OUTER_BOUND('',#1657,.T.);
#1155=FACE_OUTER_BOUND('',#1658,.T.);
#1156=FACE_OUTER_BOUND('',#1661,.T.);
#1157=FACE_OUTER_BOUND('',#1662,.T.);
#1158=FACE_OUTER_BOUND('',#1663,.T.);
#1159=FACE_OUTER_BOUND('',#1666,.T.);
#1160=FACE_OUTER_BOUND('',#1668,.T.);
#1161=FACE_OUTER_BOUND('',#1669,.T.);
#1162=FACE_OUTER_BOUND('',#1670,.T.);
#1163=FACE_OUTER_BOUND('',#1671,.T.);
#1164=FACE_OUTER_BOUND('',#1672,.T.);
#1165=FACE_OUTER_BOUND('',#1673,.T.);
#1166=FACE_OUTER_BOUND('',#1675,.T.);
#1167=FACE_OUTER_BOUND('',#1677,.T.);
#1168=FACE_OUTER_BOUND('',#1678,.T.);
#1169=FACE_OUTER_BOUND('',#1679,.T.);
#1170=FACE_OUTER_BOUND('',#1680,.T.);
#1171=FACE_OUTER_BOUND('',#1682,.T.);
#1172=FACE_OUTER_BOUND('',#1684,.T.);
#1173=FACE_OUTER_BOUND('',#1686,.T.);
#1174=FACE_OUTER_BOUND('',#1688,.T.);
#1175=FACE_OUTER_BOUND('',#1689,.T.);
#1176=FACE_OUTER_BOUND('',#1690,.T.);
#1177=FACE_OUTER_BOUND('',#1691,.T.);
#1178=FACE_OUTER_BOUND('',#1692,.T.);
#1179=FACE_OUTER_BOUND('',#1694,.T.);
#1180=FACE_OUTER_BOUND('',#1696,.T.);
#1181=FACE_OUTER_BOUND('',#1697,.T.);
#1182=FACE_OUTER_BOUND('',#1698,.T.);
#1183=FACE_OUTER_BOUND('',#1699,.T.);
#1184=FACE_OUTER_BOUND('',#1701,.T.);
#1185=FACE_OUTER_BOUND('',#1703,.T.);
#1186=FACE_OUTER_BOUND('',#1704,.T.);
#1187=FACE_OUTER_BOUND('',#1705,.T.);
#1188=FACE_OUTER_BOUND('',#1707,.T.);
#1189=FACE_OUTER_BOUND('',#1709,.T.);
#1190=FACE_OUTER_BOUND('',#1710,.T.);
#1191=FACE_OUTER_BOUND('',#1711,.T.);
#1192=FACE_OUTER_BOUND('',#1713,.T.);
#1193=FACE_OUTER_BOUND('',#1715,.T.);
#1194=FACE_OUTER_BOUND('',#1716,.T.);
#1195=FACE_OUTER_BOUND('',#1717,.T.);
#1196=FACE_OUTER_BOUND('',#1719,.T.);
#1197=FACE_OUTER_BOUND('',#1721,.T.);
#1198=FACE_OUTER_BOUND('',#1722,.T.);
#1199=FACE_OUTER_BOUND('',#1723,.T.);
#1200=FACE_OUTER_BOUND('',#1725,.T.);
#1201=FACE_OUTER_BOUND('',#1727,.T.);
#1202=FACE_OUTER_BOUND('',#1728,.T.);
#1203=FACE_OUTER_BOUND('',#1729,.T.);
#1204=FACE_OUTER_BOUND('',#1730,.T.);
#1205=FACE_OUTER_BOUND('',#1731,.T.);
#1206=FACE_OUTER_BOUND('',#1732,.T.);
#1207=FACE_OUTER_BOUND('',#1733,.T.);
#1208=FACE_OUTER_BOUND('',#1734,.T.);
#1209=FACE_OUTER_BOUND('',#1735,.T.);
#1210=FACE_OUTER_BOUND('',#1737,.T.);
#1211=FACE_OUTER_BOUND('',#1738,.T.);
#1212=FACE_OUTER_BOUND('',#1739,.T.);
#1213=FACE_OUTER_BOUND('',#1740,.T.);
#1214=FACE_OUTER_BOUND('',#1741,.T.);
#1215=FACE_OUTER_BOUND('',#1742,.T.);
#1216=FACE_OUTER_BOUND('',#1743,.T.);
#1217=FACE_OUTER_BOUND('',#1745,.T.);
#1218=FACE_OUTER_BOUND('',#1746,.T.);
#1219=FACE_OUTER_BOUND('',#1747,.T.);
#1220=FACE_OUTER_BOUND('',#1748,.T.);
#1221=FACE_OUTER_BOUND('',#1749,.T.);
#1222=FACE_OUTER_BOUND('',#1750,.T.);
#1223=FACE_OUTER_BOUND('',#1751,.T.);
#1224=FACE_OUTER_BOUND('',#1752,.T.);
#1225=FACE_OUTER_BOUND('',#1753,.T.);
#1226=FACE_OUTER_BOUND('',#1754,.T.);
#1227=FACE_OUTER_BOUND('',#1755,.T.);
#1228=FACE_OUTER_BOUND('',#1756,.T.);
#1229=FACE_OUTER_BOUND('',#1757,.T.);
#1230=FACE_OUTER_BOUND('',#1758,.T.);
#1231=FACE_OUTER_BOUND('',#1759,.T.);
#1232=FACE_OUTER_BOUND('',#1760,.T.);
#1233=FACE_OUTER_BOUND('',#1761,.T.);
#1234=FACE_OUTER_BOUND('',#1762,.T.);
#1235=FACE_OUTER_BOUND('',#1763,.T.);
#1236=FACE_OUTER_BOUND('',#1764,.T.);
#1237=FACE_OUTER_BOUND('',#1765,.T.);
#1238=FACE_OUTER_BOUND('',#1766,.T.);
#1239=FACE_OUTER_BOUND('',#1767,.T.);
#1240=FACE_OUTER_BOUND('',#1768,.T.);
#1241=FACE_OUTER_BOUND('',#1769,.T.);
#1242=FACE_OUTER_BOUND('',#1770,.T.);
#1243=FACE_OUTER_BOUND('',#1772,.T.);
#1244=FACE_OUTER_BOUND('',#1773,.T.);
#1245=FACE_OUTER_BOUND('',#1774,.T.);
#1246=FACE_OUTER_BOUND('',#1775,.T.);
#1247=FACE_OUTER_BOUND('',#1776,.T.);
#1248=FACE_OUTER_BOUND('',#1777,.T.);
#1249=FACE_OUTER_BOUND('',#1778,.T.);
#1250=FACE_OUTER_BOUND('',#1781,.T.);
#1251=FACE_OUTER_BOUND('',#1782,.T.);
#1252=FACE_OUTER_BOUND('',#1783,.T.);
#1253=FACE_OUTER_BOUND('',#1786,.T.);
#1254=FACE_OUTER_BOUND('',#1787,.T.);
#1255=FACE_OUTER_BOUND('',#1788,.T.);
#1256=FACE_OUTER_BOUND('',#1790,.T.);
#1257=FACE_OUTER_BOUND('',#1792,.T.);
#1258=FACE_OUTER_BOUND('',#1793,.T.);
#1259=FACE_OUTER_BOUND('',#1794,.T.);
#1260=FACE_OUTER_BOUND('',#1796,.T.);
#1261=EDGE_LOOP('',(#4068,#4069,#4070,#4071));
#1262=EDGE_LOOP('',(#4072,#4073,#4074,#4075));
#1263=EDGE_LOOP('',(#4076,#4077,#4078,#4079));
#1264=EDGE_LOOP('',(#4080,#4081,#4082,#4083));
#1265=EDGE_LOOP('',(#4084,#4085,#4086,#4087));
#1266=EDGE_LOOP('',(#4088,#4089,#4090,#4091));
#1267=EDGE_LOOP('',(#4092,#4093,#4094,#4095));
#1268=EDGE_LOOP('',(#4096,#4097,#4098,#4099));
#1269=EDGE_LOOP('',(#4100,#4101,#4102,#4103));
#1270=EDGE_LOOP('',(#4104,#4105,#4106,#4107));
#1271=EDGE_LOOP('',(#4108,#4109,#4110,#4111));
#1272=EDGE_LOOP('',(#4112,#4113,#4114,#4115));
#1273=EDGE_LOOP('',(#4116,#4117,#4118,#4119));
#1274=EDGE_LOOP('',(#4120));
#1275=EDGE_LOOP('',(#4121));
#1276=EDGE_LOOP('',(#4122));
#1277=EDGE_LOOP('',(#4123));
#1278=EDGE_LOOP('',(#4124));
#1279=EDGE_LOOP('',(#4125));
#1280=EDGE_LOOP('',(#4126));
#1281=EDGE_LOOP('',(#4127));
#1282=EDGE_LOOP('',(#4128,#4129,#4130,#4131));
#1283=EDGE_LOOP('',(#4132));
#1284=EDGE_LOOP('',(#4133));
#1285=EDGE_LOOP('',(#4134));
#1286=EDGE_LOOP('',(#4135));
#1287=EDGE_LOOP('',(#4136));
#1288=EDGE_LOOP('',(#4137));
#1289=EDGE_LOOP('',(#4138));
#1290=EDGE_LOOP('',(#4139));
#1291=EDGE_LOOP('',(#4140,#4141,#4142,#4143));
#1292=EDGE_LOOP('',(#4144,#4145,#4146,#4147));
#1293=EDGE_LOOP('',(#4148,#4149,#4150,#4151));
#1294=EDGE_LOOP('',(#4152,#4153,#4154,#4155));
#1295=EDGE_LOOP('',(#4156,#4157,#4158,#4159));
#1296=EDGE_LOOP('',(#4160,#4161,#4162,#4163));
#1297=EDGE_LOOP('',(#4164,#4165,#4166,#4167));
#1298=EDGE_LOOP('',(#4168,#4169,#4170,#4171));
#1299=EDGE_LOOP('',(#4172,#4173,#4174,#4175));
#1300=EDGE_LOOP('',(#4176,#4177,#4178,#4179));
#1301=EDGE_LOOP('',(#4180,#4181,#4182,#4183));
#1302=EDGE_LOOP('',(#4184,#4185,#4186,#4187));
#1303=EDGE_LOOP('',(#4188,#4189));
#1304=EDGE_LOOP('',(#4190,#4191,#4192,#4193));
#1305=EDGE_LOOP('',(#4194,#4195,#4196,#4197));
#1306=EDGE_LOOP('',(#4198,#4199));
#1307=EDGE_LOOP('',(#4200,#4201,#4202,#4203));
#1308=EDGE_LOOP('',(#4204,#4205));
#1309=EDGE_LOOP('',(#4206,#4207,#4208,#4209));
#1310=EDGE_LOOP('',(#4210,#4211));
#1311=EDGE_LOOP('',(#4212,#4213,#4214,#4215,#4216,#4217,#4218,#4219,#4220,
#4221,#4222,#4223,#4224,#4225,#4226,#4227,#4228,#4229,#4230,#4231));
#1312=EDGE_LOOP('',(#4232));
#1313=EDGE_LOOP('',(#4233,#4234,#4235,#4236,#4237,#4238,#4239,#4240,#4241));
#1314=EDGE_LOOP('',(#4242));
#1315=EDGE_LOOP('',(#4243));
#1316=EDGE_LOOP('',(#4244));
#1317=EDGE_LOOP('',(#4245));
#1318=EDGE_LOOP('',(#4246,#4247,#4248,#4249));
#1319=EDGE_LOOP('',(#4250));
#1320=EDGE_LOOP('',(#4251,#4252,#4253,#4254));
#1321=EDGE_LOOP('',(#4255));
#1322=EDGE_LOOP('',(#4256,#4257,#4258,#4259));
#1323=EDGE_LOOP('',(#4260));
#1324=EDGE_LOOP('',(#4261,#4262,#4263,#4264));
#1325=EDGE_LOOP('',(#4265));
#1326=EDGE_LOOP('',(#4266,#4267,#4268,#4269,#4270,#4271));
#1327=EDGE_LOOP('',(#4272,#4273,#4274,#4275));
#1328=EDGE_LOOP('',(#4276,#4277,#4278,#4279));
#1329=EDGE_LOOP('',(#4280,#4281,#4282,#4283));
#1330=EDGE_LOOP('',(#4284,#4285,#4286,#4287));
#1331=EDGE_LOOP('',(#4288,#4289,#4290,#4291));
#1332=EDGE_LOOP('',(#4292));
#1333=EDGE_LOOP('',(#4293));
#1334=EDGE_LOOP('',(#4294,#4295,#4296,#4297));
#1335=EDGE_LOOP('',(#4298,#4299));
#1336=EDGE_LOOP('',(#4300,#4301,#4302,#4303));
#1337=EDGE_LOOP('',(#4304,#4305));
#1338=EDGE_LOOP('',(#4306));
#1339=EDGE_LOOP('',(#4307));
#1340=EDGE_LOOP('',(#4308));
#1341=EDGE_LOOP('',(#4309));
#1342=EDGE_LOOP('',(#4310));
#1343=EDGE_LOOP('',(#4311));
#1344=EDGE_LOOP('',(#4312));
#1345=EDGE_LOOP('',(#4313));
#1346=EDGE_LOOP('',(#4314));
#1347=EDGE_LOOP('',(#4315));
#1348=EDGE_LOOP('',(#4316));
#1349=EDGE_LOOP('',(#4317));
#1350=EDGE_LOOP('',(#4318,#4319,#4320,#4321));
#1351=EDGE_LOOP('',(#4322,#4323,#4324,#4325));
#1352=EDGE_LOOP('',(#4326));
#1353=EDGE_LOOP('',(#4327));
#1354=EDGE_LOOP('',(#4328));
#1355=EDGE_LOOP('',(#4329));
#1356=EDGE_LOOP('',(#4330,#4331,#4332,#4333));
#1357=EDGE_LOOP('',(#4334,#4335,#4336,#4337));
#1358=EDGE_LOOP('',(#4338,#4339,#4340,#4341));
#1359=EDGE_LOOP('',(#4342,#4343,#4344,#4345));
#1360=EDGE_LOOP('',(#4346,#4347,#4348,#4349));
#1361=EDGE_LOOP('',(#4350));
#1362=EDGE_LOOP('',(#4351));
#1363=EDGE_LOOP('',(#4352,#4353,#4354,#4355));
#1364=EDGE_LOOP('',(#4356,#4357,#4358,#4359));
#1365=EDGE_LOOP('',(#4360));
#1366=EDGE_LOOP('',(#4361));
#1367=EDGE_LOOP('',(#4362));
#1368=EDGE_LOOP('',(#4363));
#1369=EDGE_LOOP('',(#4364));
#1370=EDGE_LOOP('',(#4365));
#1371=EDGE_LOOP('',(#4366));
#1372=EDGE_LOOP('',(#4367));
#1373=EDGE_LOOP('',(#4368));
#1374=EDGE_LOOP('',(#4369));
#1375=EDGE_LOOP('',(#4370));
#1376=EDGE_LOOP('',(#4371));
#1377=EDGE_LOOP('',(#4372,#4373));
#1378=EDGE_LOOP('',(#4374,#4375,#4376,#4377));
#1379=EDGE_LOOP('',(#4378,#4379,#4380,#4381));
#1380=EDGE_LOOP('',(#4382,#4383));
#1381=EDGE_LOOP('',(#4384,#4385,#4386,#4387));
#1382=EDGE_LOOP('',(#4388,#4389));
#1383=EDGE_LOOP('',(#4390,#4391,#4392,#4393));
#1384=EDGE_LOOP('',(#4394,#4395));
#1385=EDGE_LOOP('',(#4396,#4397,#4398,#4399,#4400,#4401,#4402,#4403,#4404,
#4405,#4406,#4407,#4408,#4409,#4410,#4411,#4412,#4413,#4414,#4415));
#1386=EDGE_LOOP('',(#4416));
#1387=EDGE_LOOP('',(#4417,#4418,#4419,#4420,#4421,#4422,#4423,#4424,#4425));
#1388=EDGE_LOOP('',(#4426));
#1389=EDGE_LOOP('',(#4427));
#1390=EDGE_LOOP('',(#4428));
#1391=EDGE_LOOP('',(#4429));
#1392=EDGE_LOOP('',(#4430,#4431,#4432,#4433));
#1393=EDGE_LOOP('',(#4434));
#1394=EDGE_LOOP('',(#4435,#4436,#4437,#4438));
#1395=EDGE_LOOP('',(#4439));
#1396=EDGE_LOOP('',(#4440,#4441,#4442,#4443));
#1397=EDGE_LOOP('',(#4444));
#1398=EDGE_LOOP('',(#4445,#4446,#4447,#4448));
#1399=EDGE_LOOP('',(#4449));
#1400=EDGE_LOOP('',(#4450,#4451,#4452,#4453,#4454,#4455));
#1401=EDGE_LOOP('',(#4456,#4457,#4458,#4459));
#1402=EDGE_LOOP('',(#4460,#4461,#4462,#4463));
#1403=EDGE_LOOP('',(#4464,#4465,#4466,#4467));
#1404=EDGE_LOOP('',(#4468,#4469,#4470,#4471));
#1405=EDGE_LOOP('',(#4472,#4473,#4474,#4475));
#1406=EDGE_LOOP('',(#4476));
#1407=EDGE_LOOP('',(#4477));
#1408=EDGE_LOOP('',(#4478,#4479,#4480,#4481));
#1409=EDGE_LOOP('',(#4482,#4483));
#1410=EDGE_LOOP('',(#4484,#4485,#4486,#4487));
#1411=EDGE_LOOP('',(#4488,#4489));
#1412=EDGE_LOOP('',(#4490));
#1413=EDGE_LOOP('',(#4491));
#1414=EDGE_LOOP('',(#4492));
#1415=EDGE_LOOP('',(#4493));
#1416=EDGE_LOOP('',(#4494));
#1417=EDGE_LOOP('',(#4495));
#1418=EDGE_LOOP('',(#4496));
#1419=EDGE_LOOP('',(#4497));
#1420=EDGE_LOOP('',(#4498));
#1421=EDGE_LOOP('',(#4499));
#1422=EDGE_LOOP('',(#4500));
#1423=EDGE_LOOP('',(#4501));
#1424=EDGE_LOOP('',(#4502,#4503,#4504,#4505));
#1425=EDGE_LOOP('',(#4506,#4507,#4508,#4509));
#1426=EDGE_LOOP('',(#4510,#4511,#4512,#4513));
#1427=EDGE_LOOP('',(#4514,#4515,#4516,#4517));
#1428=EDGE_LOOP('',(#4518,#4519,#4520,#4521));
#1429=EDGE_LOOP('',(#4522));
#1430=EDGE_LOOP('',(#4523));
#1431=EDGE_LOOP('',(#4524,#4525,#4526,#4527));
#1432=EDGE_LOOP('',(#4528,#4529,#4530,#4531));
#1433=EDGE_LOOP('',(#4532));
#1434=EDGE_LOOP('',(#4533));
#1435=EDGE_LOOP('',(#4534));
#1436=EDGE_LOOP('',(#4535));
#1437=EDGE_LOOP('',(#4536));
#1438=EDGE_LOOP('',(#4537));
#1439=EDGE_LOOP('',(#4538));
#1440=EDGE_LOOP('',(#4539));
#1441=EDGE_LOOP('',(#4540));
#1442=EDGE_LOOP('',(#4541));
#1443=EDGE_LOOP('',(#4542));
#1444=EDGE_LOOP('',(#4543));
#1445=EDGE_LOOP('',(#4544,#4545,#4546,#4547));
#1446=EDGE_LOOP('',(#4548,#4549,#4550,#4551));
#1447=EDGE_LOOP('',(#4552,#4553,#4554,#4555));
#1448=EDGE_LOOP('',(#4556,#4557,#4558,#4559));
#1449=EDGE_LOOP('',(#4560,#4561,#4562,#4563));
#1450=EDGE_LOOP('',(#4564,#4565,#4566,#4567));
#1451=EDGE_LOOP('',(#4568,#4569,#4570,#4571,#4572,#4573));
#1452=EDGE_LOOP('',(#4574,#4575,#4576,#4577,#4578,#4579));
#1453=EDGE_LOOP('',(#4580));
#1454=EDGE_LOOP('',(#4581));
#1455=EDGE_LOOP('',(#4582,#4583,#4584,#4585));
#1456=EDGE_LOOP('',(#4586,#4587,#4588,#4589));
#1457=EDGE_LOOP('',(#4590,#4591,#4592,#4593));
#1458=EDGE_LOOP('',(#4594));
#1459=EDGE_LOOP('',(#4595));
#1460=EDGE_LOOP('',(#4596,#4597,#4598,#4599));
#1461=EDGE_LOOP('',(#4600,#4601,#4602,#4603));
#1462=EDGE_LOOP('',(#4604,#4605,#4606,#4607,#4608,#4609));
#1463=EDGE_LOOP('',(#4610,#4611,#4612,#4613,#4614));
#1464=EDGE_LOOP('',(#4615,#4616,#4617,#4618));
#1465=EDGE_LOOP('',(#4619,#4620,#4621,#4622));
#1466=EDGE_LOOP('',(#4623));
#1467=EDGE_LOOP('',(#4624));
#1468=EDGE_LOOP('',(#4625,#4626,#4627,#4628,#4629));
#1469=EDGE_LOOP('',(#4630));
#1470=EDGE_LOOP('',(#4631));
#1471=EDGE_LOOP('',(#4632,#4633,#4634,#4635));
#1472=EDGE_LOOP('',(#4636,#4637,#4638,#4639,#4640,#4641));
#1473=EDGE_LOOP('',(#4642,#4643,#4644,#4645,#4646));
#1474=EDGE_LOOP('',(#4647));
#1475=EDGE_LOOP('',(#4648));
#1476=EDGE_LOOP('',(#4649,#4650,#4651,#4652));
#1477=EDGE_LOOP('',(#4653,#4654,#4655,#4656));
#1478=EDGE_LOOP('',(#4657,#4658,#4659,#4660));
#1479=EDGE_LOOP('',(#4661));
#1480=EDGE_LOOP('',(#4662));
#1481=EDGE_LOOP('',(#4663,#4664,#4665,#4666,#4667));
#1482=EDGE_LOOP('',(#4668,#4669));
#1483=EDGE_LOOP('',(#4670,#4671));
#1484=EDGE_LOOP('',(#4672,#4673));
#1485=EDGE_LOOP('',(#4674,#4675));
#1486=EDGE_LOOP('',(#4676,#4677));
#1487=EDGE_LOOP('',(#4678,#4679));
#1488=EDGE_LOOP('',(#4680,#4681));
#1489=EDGE_LOOP('',(#4682,#4683));
#1490=EDGE_LOOP('',(#4684,#4685,#4686,#4687));
#1491=EDGE_LOOP('',(#4688,#4689,#4690,#4691,#4692,#4693,#4694,#4695,#4696,
#4697,#4698,#4699,#4700,#4701,#4702,#4703,#4704,#4705,#4706,#4707));
#1492=EDGE_LOOP('',(#4708,#4709,#4710,#4711));
#1493=EDGE_LOOP('',(#4712,#4713,#4714,#4715));
#1494=EDGE_LOOP('',(#4716,#4717,#4718,#4719));
#1495=EDGE_LOOP('',(#4720,#4721,#4722,#4723));
#1496=EDGE_LOOP('',(#4724,#4725,#4726,#4727));
#1497=EDGE_LOOP('',(#4728,#4729,#4730,#4731,#4732,#4733));
#1498=EDGE_LOOP('',(#4734,#4735,#4736,#4737));
#1499=EDGE_LOOP('',(#4738,#4739,#4740,#4741));
#1500=EDGE_LOOP('',(#4742,#4743,#4744,#4745));
#1501=EDGE_LOOP('',(#4746,#4747,#4748,#4749));
#1502=EDGE_LOOP('',(#4750,#4751,#4752,#4753));
#1503=EDGE_LOOP('',(#4754,#4755,#4756,#4757));
#1504=EDGE_LOOP('',(#4758,#4759,#4760,#4761,#4762,#4763,#4764,#4765,#4766,
#4767,#4768,#4769,#4770,#4771,#4772,#4773,#4774,#4775,#4776,#4777));
#1505=EDGE_LOOP('',(#4778,#4779,#4780,#4781));
#1506=EDGE_LOOP('',(#4782,#4783,#4784,#4785));
#1507=EDGE_LOOP('',(#4786));
#1508=EDGE_LOOP('',(#4787));
#1509=EDGE_LOOP('',(#4788,#4789,#4790,#4791));
#1510=EDGE_LOOP('',(#4792));
#1511=EDGE_LOOP('',(#4793));
#1512=EDGE_LOOP('',(#4794,#4795,#4796,#4797));
#1513=EDGE_LOOP('',(#4798));
#1514=EDGE_LOOP('',(#4799));
#1515=EDGE_LOOP('',(#4800,#4801,#4802,#4803));
#1516=EDGE_LOOP('',(#4804));
#1517=EDGE_LOOP('',(#4805));
#1518=EDGE_LOOP('',(#4806,#4807,#4808,#4809));
#1519=EDGE_LOOP('',(#4810));
#1520=EDGE_LOOP('',(#4811));
#1521=EDGE_LOOP('',(#4812,#4813,#4814,#4815));
#1522=EDGE_LOOP('',(#4816,#4817,#4818,#4819));
#1523=EDGE_LOOP('',(#4820));
#1524=EDGE_LOOP('',(#4821,#4822,#4823,#4824));
#1525=EDGE_LOOP('',(#4825,#4826,#4827,#4828));
#1526=EDGE_LOOP('',(#4829,#4830,#4831,#4832));
#1527=EDGE_LOOP('',(#4833,#4834,#4835,#4836));
#1528=EDGE_LOOP('',(#4837));
#1529=EDGE_LOOP('',(#4838));
#1530=EDGE_LOOP('',(#4839,#4840,#4841,#4842));
#1531=EDGE_LOOP('',(#4843,#4844,#4845,#4846));
#1532=EDGE_LOOP('',(#4847,#4848,#4849,#4850));
#1533=EDGE_LOOP('',(#4851));
#1534=EDGE_LOOP('',(#4852));
#1535=EDGE_LOOP('',(#4853));
#1536=EDGE_LOOP('',(#4854));
#1537=EDGE_LOOP('',(#4855,#4856,#4857,#4858));
#1538=EDGE_LOOP('',(#4859,#4860,#4861,#4862));
#1539=EDGE_LOOP('',(#4863,#4864,#4865,#4866));
#1540=EDGE_LOOP('',(#4867));
#1541=EDGE_LOOP('',(#4868));
#1542=EDGE_LOOP('',(#4869));
#1543=EDGE_LOOP('',(#4870,#4871,#4872,#4873));
#1544=EDGE_LOOP('',(#4874,#4875,#4876,#4877));
#1545=EDGE_LOOP('',(#4878));
#1546=EDGE_LOOP('',(#4879));
#1547=EDGE_LOOP('',(#4880));
#1548=EDGE_LOOP('',(#4881));
#1549=EDGE_LOOP('',(#4882,#4883,#4884,#4885));
#1550=EDGE_LOOP('',(#4886,#4887,#4888,#4889));
#1551=EDGE_LOOP('',(#4890));
#1552=EDGE_LOOP('',(#4891));
#1553=EDGE_LOOP('',(#4892));
#1554=EDGE_LOOP('',(#4893));
#1555=EDGE_LOOP('',(#4894,#4895));
#1556=EDGE_LOOP('',(#4896,#4897,#4898,#4899,#4900,#4901,#4902,#4903,#4904));
#1557=EDGE_LOOP('',(#4905,#4906));
#1558=EDGE_LOOP('',(#4907,#4908,#4909,#4910));
#1559=EDGE_LOOP('',(#4911,#4912,#4913,#4914,#4915));
#1560=EDGE_LOOP('',(#4916,#4917,#4918,#4919));
#1561=EDGE_LOOP('',(#4920,#4921));
#1562=EDGE_LOOP('',(#4922));
#1563=EDGE_LOOP('',(#4923));
#1564=EDGE_LOOP('',(#4924));
#1565=EDGE_LOOP('',(#4925));
#1566=EDGE_LOOP('',(#4926,#4927));
#1567=EDGE_LOOP('',(#4928,#4929,#4930,#4931,#4932,#4933,#4934,#4935,#4936));
#1568=EDGE_LOOP('',(#4937,#4938));
#1569=EDGE_LOOP('',(#4939,#4940,#4941,#4942));
#1570=EDGE_LOOP('',(#4943,#4944,#4945,#4946,#4947));
#1571=EDGE_LOOP('',(#4948,#4949,#4950,#4951));
#1572=EDGE_LOOP('',(#4952,#4953));
#1573=EDGE_LOOP('',(#4954));
#1574=EDGE_LOOP('',(#4955));
#1575=EDGE_LOOP('',(#4956));
#1576=EDGE_LOOP('',(#4957));
#1577=EDGE_LOOP('',(#4958,#4959,#4960,#4961));
#1578=EDGE_LOOP('',(#4962,#4963,#4964,#4965));
#1579=EDGE_LOOP('',(#4966));
#1580=EDGE_LOOP('',(#4967));
#1581=EDGE_LOOP('',(#4968));
#1582=EDGE_LOOP('',(#4969));
#1583=EDGE_LOOP('',(#4970,#4971,#4972,#4973));
#1584=EDGE_LOOP('',(#4974));
#1585=EDGE_LOOP('',(#4975,#4976,#4977,#4978));
#1586=EDGE_LOOP('',(#4979));
#1587=EDGE_LOOP('',(#4980));
#1588=EDGE_LOOP('',(#4981));
#1589=EDGE_LOOP('',(#4982));
#1590=EDGE_LOOP('',(#4983));
#1591=EDGE_LOOP('',(#4984,#4985,#4986,#4987));
#1592=EDGE_LOOP('',(#4988,#4989,#4990,#4991));
#1593=EDGE_LOOP('',(#4992,#4993,#4994,#4995));
#1594=EDGE_LOOP('',(#4996));
#1595=EDGE_LOOP('',(#4997));
#1596=EDGE_LOOP('',(#4998));
#1597=EDGE_LOOP('',(#4999));
#1598=EDGE_LOOP('',(#5000,#5001,#5002,#5003));
#1599=EDGE_LOOP('',(#5004,#5005,#5006,#5007));
#1600=EDGE_LOOP('',(#5008));
#1601=EDGE_LOOP('',(#5009));
#1602=EDGE_LOOP('',(#5010));
#1603=EDGE_LOOP('',(#5011));
#1604=EDGE_LOOP('',(#5012,#5013,#5014,#5015));
#1605=EDGE_LOOP('',(#5016,#5017,#5018,#5019));
#1606=EDGE_LOOP('',(#5020));
#1607=EDGE_LOOP('',(#5021));
#1608=EDGE_LOOP('',(#5022));
#1609=EDGE_LOOP('',(#5023));
#1610=EDGE_LOOP('',(#5024,#5025,#5026,#5027));
#1611=EDGE_LOOP('',(#5028,#5029,#5030,#5031));
#1612=EDGE_LOOP('',(#5032));
#1613=EDGE_LOOP('',(#5033));
#1614=EDGE_LOOP('',(#5034));
#1615=EDGE_LOOP('',(#5035));
#1616=EDGE_LOOP('',(#5036,#5037,#5038,#5039));
#1617=EDGE_LOOP('',(#5040,#5041,#5042,#5043));
#1618=EDGE_LOOP('',(#5044));
#1619=EDGE_LOOP('',(#5045));
#1620=EDGE_LOOP('',(#5046));
#1621=EDGE_LOOP('',(#5047));
#1622=EDGE_LOOP('',(#5048,#5049,#5050,#5051));
#1623=EDGE_LOOP('',(#5052,#5053,#5054,#5055));
#1624=EDGE_LOOP('',(#5056,#5057,#5058,#5059));
#1625=EDGE_LOOP('',(#5060,#5061,#5062,#5063));
#1626=EDGE_LOOP('',(#5064,#5065,#5066,#5067));
#1627=EDGE_LOOP('',(#5068,#5069,#5070,#5071));
#1628=EDGE_LOOP('',(#5072,#5073,#5074,#5075,#5076,#5077));
#1629=EDGE_LOOP('',(#5078));
#1630=EDGE_LOOP('',(#5079,#5080,#5081,#5082,#5083,#5084));
#1631=EDGE_LOOP('',(#5085,#5086,#5087,#5088));
#1632=EDGE_LOOP('',(#5089,#5090,#5091,#5092));
#1633=EDGE_LOOP('',(#5093,#5094,#5095,#5096));
#1634=EDGE_LOOP('',(#5097));
#1635=EDGE_LOOP('',(#5098,#5099,#5100,#5101));
#1636=EDGE_LOOP('',(#5102,#5103,#5104,#5105));
#1637=EDGE_LOOP('',(#5106,#5107,#5108,#5109));
#1638=EDGE_LOOP('',(#5110,#5111,#5112,#5113));
#1639=EDGE_LOOP('',(#5114,#5115,#5116,#5117));
#1640=EDGE_LOOP('',(#5118));
#1641=EDGE_LOOP('',(#5119));
#1642=EDGE_LOOP('',(#5120));
#1643=EDGE_LOOP('',(#5121));
#1644=EDGE_LOOP('',(#5122));
#1645=EDGE_LOOP('',(#5123,#5124,#5125,#5126));
#1646=EDGE_LOOP('',(#5127,#5128,#5129,#5130));
#1647=EDGE_LOOP('',(#5131,#5132,#5133,#5134));
#1648=EDGE_LOOP('',(#5135,#5136,#5137,#5138));
#1649=EDGE_LOOP('',(#5139,#5140,#5141,#5142));
#1650=EDGE_LOOP('',(#5143));
#1651=EDGE_LOOP('',(#5144));
#1652=EDGE_LOOP('',(#5145));
#1653=EDGE_LOOP('',(#5146));
#1654=EDGE_LOOP('',(#5147,#5148,#5149,#5150));
#1655=EDGE_LOOP('',(#5151,#5152,#5153,#5154));
#1656=EDGE_LOOP('',(#5155,#5156,#5157,#5158));
#1657=EDGE_LOOP('',(#5159,#5160,#5161,#5162));
#1658=EDGE_LOOP('',(#5163,#5164,#5165,#5166));
#1659=EDGE_LOOP('',(#5167));
#1660=EDGE_LOOP('',(#5168));
#1661=EDGE_LOOP('',(#5169,#5170,#5171,#5172));
#1662=EDGE_LOOP('',(#5173,#5174,#5175,#5176));
#1663=EDGE_LOOP('',(#5177,#5178,#5179,#5180));
#1664=EDGE_LOOP('',(#5181));
#1665=EDGE_LOOP('',(#5182));
#1666=EDGE_LOOP('',(#5183));
#1667=EDGE_LOOP('',(#5184));
#1668=EDGE_LOOP('',(#5185,#5186,#5187,#5188));
#1669=EDGE_LOOP('',(#5189,#5190,#5191,#5192));
#1670=EDGE_LOOP('',(#5193));
#1671=EDGE_LOOP('',(#5194,#5195,#5196,#5197));
#1672=EDGE_LOOP('',(#5198,#5199,#5200,#5201));
#1673=EDGE_LOOP('',(#5202));
#1674=EDGE_LOOP('',(#5203));
#1675=EDGE_LOOP('',(#5204));
#1676=EDGE_LOOP('',(#5205));
#1677=EDGE_LOOP('',(#5206,#5207));
#1678=EDGE_LOOP('',(#5208,#5209,#5210,#5211,#5212,#5213,#5214,#5215,#5216));
#1679=EDGE_LOOP('',(#5217,#5218));
#1680=EDGE_LOOP('',(#5219,#5220,#5221,#5222));
#1681=EDGE_LOOP('',(#5223,#5224,#5225,#5226,#5227));
#1682=EDGE_LOOP('',(#5228,#5229,#5230,#5231));
#1683=EDGE_LOOP('',(#5232,#5233));
#1684=EDGE_LOOP('',(#5234));
#1685=EDGE_LOOP('',(#5235));
#1686=EDGE_LOOP('',(#5236));
#1687=EDGE_LOOP('',(#5237));
#1688=EDGE_LOOP('',(#5238,#5239,#5240,#5241));
#1689=EDGE_LOOP('',(#5242));
#1690=EDGE_LOOP('',(#5243,#5244,#5245,#5246));
#1691=EDGE_LOOP('',(#5247));
#1692=EDGE_LOOP('',(#5248));
#1693=EDGE_LOOP('',(#5249));
#1694=EDGE_LOOP('',(#5250));
#1695=EDGE_LOOP('',(#5251));
#1696=EDGE_LOOP('',(#5252,#5253,#5254,#5255));
#1697=EDGE_LOOP('',(#5256,#5257,#5258,#5259));
#1698=EDGE_LOOP('',(#5260,#5261,#5262,#5263));
#1699=EDGE_LOOP('',(#5264));
#1700=EDGE_LOOP('',(#5265));
#1701=EDGE_LOOP('',(#5266));
#1702=EDGE_LOOP('',(#5267));
#1703=EDGE_LOOP('',(#5268,#5269,#5270,#5271));
#1704=EDGE_LOOP('',(#5272,#5273,#5274,#5275));
#1705=EDGE_LOOP('',(#5276));
#1706=EDGE_LOOP('',(#5277));
#1707=EDGE_LOOP('',(#5278));
#1708=EDGE_LOOP('',(#5279));
#1709=EDGE_LOOP('',(#5280,#5281,#5282,#5283));
#1710=EDGE_LOOP('',(#5284,#5285,#5286,#5287));
#1711=EDGE_LOOP('',(#5288));
#1712=EDGE_LOOP('',(#5289));
#1713=EDGE_LOOP('',(#5290));
#1714=EDGE_LOOP('',(#5291));
#1715=EDGE_LOOP('',(#5292,#5293,#5294,#5295));
#1716=EDGE_LOOP('',(#5296,#5297,#5298,#5299));
#1717=EDGE_LOOP('',(#5300));
#1718=EDGE_LOOP('',(#5301));
#1719=EDGE_LOOP('',(#5302));
#1720=EDGE_LOOP('',(#5303));
#1721=EDGE_LOOP('',(#5304,#5305,#5306,#5307));
#1722=EDGE_LOOP('',(#5308,#5309,#5310,#5311));
#1723=EDGE_LOOP('',(#5312));
#1724=EDGE_LOOP('',(#5313));
#1725=EDGE_LOOP('',(#5314));
#1726=EDGE_LOOP('',(#5315));
#1727=EDGE_LOOP('',(#5316));
#1728=EDGE_LOOP('',(#5317,#5318,#5319,#5320));
#1729=EDGE_LOOP('',(#5321,#5322,#5323,#5324));
#1730=EDGE_LOOP('',(#5325,#5326,#5327,#5328));
#1731=EDGE_LOOP('',(#5329,#5330,#5331,#5332));
#1732=EDGE_LOOP('',(#5333,#5334,#5335,#5336));
#1733=EDGE_LOOP('',(#5337,#5338,#5339,#5340));
#1734=EDGE_LOOP('',(#5341,#5342,#5343,#5344,#5345,#5346));
#1735=EDGE_LOOP('',(#5347));
#1736=EDGE_LOOP('',(#5348,#5349,#5350,#5351,#5352,#5353));
#1737=EDGE_LOOP('',(#5354,#5355,#5356,#5357));
#1738=EDGE_LOOP('',(#5358,#5359,#5360,#5361));
#1739=EDGE_LOOP('',(#5362));
#1740=EDGE_LOOP('',(#5363,#5364,#5365,#5366));
#1741=EDGE_LOOP('',(#5367,#5368,#5369,#5370));
#1742=EDGE_LOOP('',(#5371,#5372,#5373,#5374));
#1743=EDGE_LOOP('',(#5375));
#1744=EDGE_LOOP('',(#5376));
#1745=EDGE_LOOP('',(#5377,#5378,#5379,#5380));
#1746=EDGE_LOOP('',(#5381,#5382,#5383,#5384));
#1747=EDGE_LOOP('',(#5385,#5386,#5387,#5388));
#1748=EDGE_LOOP('',(#5389));
#1749=EDGE_LOOP('',(#5390,#5391,#5392,#5393));
#1750=EDGE_LOOP('',(#5394,#5395,#5396,#5397));
#1751=EDGE_LOOP('',(#5398,#5399,#5400,#5401));
#1752=EDGE_LOOP('',(#5402,#5403,#5404,#5405));
#1753=EDGE_LOOP('',(#5406,#5407,#5408,#5409));
#1754=EDGE_LOOP('',(#5410,#5411,#5412,#5413));
#1755=EDGE_LOOP('',(#5414,#5415,#5416,#5417,#5418,#5419));
#1756=EDGE_LOOP('',(#5420,#5421,#5422,#5423,#5424,#5425));
#1757=EDGE_LOOP('',(#5426,#5427,#5428,#5429));
#1758=EDGE_LOOP('',(#5430,#5431,#5432,#5433));
#1759=EDGE_LOOP('',(#5434,#5435,#5436,#5437));
#1760=EDGE_LOOP('',(#5438,#5439,#5440,#5441));
#1761=EDGE_LOOP('',(#5442,#5443,#5444,#5445));
#1762=EDGE_LOOP('',(#5446,#5447,#5448,#5449));
#1763=EDGE_LOOP('',(#5450,#5451,#5452,#5453,#5454,#5455));
#1764=EDGE_LOOP('',(#5456,#5457,#5458,#5459,#5460,#5461));
#1765=EDGE_LOOP('',(#5462));
#1766=EDGE_LOOP('',(#5463));
#1767=EDGE_LOOP('',(#5464,#5465,#5466,#5467));
#1768=EDGE_LOOP('',(#5468,#5469,#5470,#5471));
#1769=EDGE_LOOP('',(#5472,#5473,#5474,#5475));
#1770=EDGE_LOOP('',(#5476));
#1771=EDGE_LOOP('',(#5477));
#1772=EDGE_LOOP('',(#5478,#5479,#5480,#5481));
#1773=EDGE_LOOP('',(#5482,#5483,#5484,#5485));
#1774=EDGE_LOOP('',(#5486,#5487,#5488,#5489));
#1775=EDGE_LOOP('',(#5490,#5491,#5492,#5493));
#1776=EDGE_LOOP('',(#5494,#5495,#5496,#5497));
#1777=EDGE_LOOP('',(#5498,#5499,#5500,#5501));
#1778=EDGE_LOOP('',(#5502,#5503,#5504,#5505));
#1779=EDGE_LOOP('',(#5506));
#1780=EDGE_LOOP('',(#5507));
#1781=EDGE_LOOP('',(#5508,#5509,#5510,#5511));
#1782=EDGE_LOOP('',(#5512,#5513,#5514,#5515));
#1783=EDGE_LOOP('',(#5516,#5517,#5518,#5519));
#1784=EDGE_LOOP('',(#5520));
#1785=EDGE_LOOP('',(#5521));
#1786=EDGE_LOOP('',(#5522,#5523,#5524,#5525));
#1787=EDGE_LOOP('',(#5526,#5527,#5528,#5529));
#1788=EDGE_LOOP('',(#5530));
#1789=EDGE_LOOP('',(#5531));
#1790=EDGE_LOOP('',(#5532));
#1791=EDGE_LOOP('',(#5533));
#1792=EDGE_LOOP('',(#5534,#5535,#5536,#5537));
#1793=EDGE_LOOP('',(#5538,#5539,#5540,#5541));
#1794=EDGE_LOOP('',(#5542));
#1795=EDGE_LOOP('',(#5543));
#1796=EDGE_LOOP('',(#5544));
#1797=EDGE_LOOP('',(#5545));
#1798=LINE('',#9455,#2131);
#1799=LINE('',#9461,#2132);
#1800=LINE('',#9467,#2133);
#1801=LINE('',#9473,#2134);
#1802=LINE('',#9479,#2135);
#1803=LINE('',#9485,#2136);
#1804=LINE('',#9491,#2137);
#1805=LINE('',#9497,#2138);
#1806=LINE('',#9502,#2139);
#1807=LINE('',#9504,#2140);
#1808=LINE('',#9506,#2141);
#1809=LINE('',#9507,#2142);
#1810=LINE('',#9510,#2143);
#1811=LINE('',#9512,#2144);
#1812=LINE('',#9513,#2145);
#1813=LINE('',#9516,#2146);
#1814=LINE('',#9518,#2147);
#1815=LINE('',#9519,#2148);
#1816=LINE('',#9521,#2149);
#1817=LINE('',#9522,#2150);
#1818=LINE('',#9529,#2151);
#1819=LINE('',#9531,#2152);
#1820=LINE('',#9533,#2153);
#1821=LINE('',#9534,#2154);
#1822=LINE('',#9537,#2155);
#1823=LINE('',#9539,#2156);
#1824=LINE('',#9540,#2157);
#1825=LINE('',#9543,#2158);
#1826=LINE('',#9545,#2159);
#1827=LINE('',#9546,#2160);
#1828=LINE('',#9548,#2161);
#1829=LINE('',#9549,#2162);
#1830=LINE('',#9556,#2163);
#1831=LINE('',#9558,#2164);
#1832=LINE('',#9560,#2165);
#1833=LINE('',#9561,#2166);
#1834=LINE('',#9564,#2167);
#1835=LINE('',#9566,#2168);
#1836=LINE('',#9567,#2169);
#1837=LINE('',#9570,#2170);
#1838=LINE('',#9572,#2171);
#1839=LINE('',#9573,#2172);
#1840=LINE('',#9575,#2173);
#1841=LINE('',#9576,#2174);
#1842=LINE('',#9587,#2175);
#1843=LINE('',#9590,#2176);
#1844=LINE('',#9594,#2177);
#1845=LINE('',#9598,#2178);
#1846=LINE('',#9605,#2179);
#1847=LINE('',#9609,#2180);
#1848=LINE('',#9616,#2181);
#1849=LINE('',#9620,#2182);
#1850=LINE('',#9628,#2183);
#1851=LINE('',#9649,#2184);
#1852=LINE('',#9656,#2185);
#1853=LINE('',#9663,#2186);
#1854=LINE('',#9670,#2187);
#1855=LINE('',#9713,#2188);
#1856=LINE('',#9754,#2189);
#1857=LINE('',#9758,#2190);
#1858=LINE('',#9762,#2191);
#1859=LINE('',#9766,#2192);
#1860=LINE('',#9771,#2193);
#1861=LINE('',#9778,#2194);
#1862=LINE('',#9782,#2195);
#1863=LINE('',#9791,#2196);
#1864=LINE('',#9797,#2197);
#1865=LINE('',#9806,#2198);
#1866=LINE('',#9812,#2199);
#1867=LINE('',#9818,#2200);
#1868=LINE('',#9824,#2201);
#1869=LINE('',#9830,#2202);
#1870=LINE('',#9838,#2203);
#1871=LINE('',#9843,#2204);
#1872=LINE('',#9855,#2205);
#1873=LINE('',#9858,#2206);
#1874=LINE('',#9862,#2207);
#1875=LINE('',#9866,#2208);
#1876=LINE('',#9873,#2209);
#1877=LINE('',#9877,#2210);
#1878=LINE('',#9884,#2211);
#1879=LINE('',#9888,#2212);
#1880=LINE('',#9896,#2213);
#1881=LINE('',#9917,#2214);
#1882=LINE('',#9924,#2215);
#1883=LINE('',#9931,#2216);
#1884=LINE('',#9938,#2217);
#1885=LINE('',#9981,#2218);
#1886=LINE('',#10022,#2219);
#1887=LINE('',#10026,#2220);
#1888=LINE('',#10030,#2221);
#1889=LINE('',#10034,#2222);
#1890=LINE('',#10039,#2223);
#1891=LINE('',#10046,#2224);
#1892=LINE('',#10050,#2225);
#1893=LINE('',#10059,#2226);
#1894=LINE('',#10065,#2227);
#1895=LINE('',#10071,#2228);
#1896=LINE('',#10077,#2229);
#1897=LINE('',#10083,#2230);
#1898=LINE('',#10091,#2231);
#1899=LINE('',#10096,#2232);
#1900=LINE('',#10104,#2233);
#1901=LINE('',#10106,#2234);
#1902=LINE('',#10108,#2235);
#1903=LINE('',#10109,#2236);
#1904=LINE('',#10112,#2237);
#1905=LINE('',#10114,#2238);
#1906=LINE('',#10115,#2239);
#1907=LINE('',#10118,#2240);
#1908=LINE('',#10120,#2241);
#1909=LINE('',#10121,#2242);
#1910=LINE('',#10124,#2243);
#1911=LINE('',#10126,#2244);
#1912=LINE('',#10127,#2245);
#1913=LINE('',#10130,#2246);
#1914=LINE('',#10132,#2247);
#1915=LINE('',#10133,#2248);
#1916=LINE('',#10135,#2249);
#1917=LINE('',#10136,#2250);
#1918=LINE('',#10148,#2251);
#1919=LINE('',#10152,#2252);
#1920=LINE('',#10156,#2253);
#1921=LINE('',#10163,#2254);
#1922=LINE('',#10165,#2255);
#1923=LINE('',#10180,#2256);
#1924=LINE('',#10186,#2257);
#1925=LINE('',#10190,#2258);
#1926=LINE('',#10196,#2259);
#1927=LINE('',#10201,#2260);
#1928=LINE('',#10216,#2261);
#1929=LINE('',#10225,#2262);
#1930=LINE('',#10229,#2263);
#1931=LINE('',#10233,#2264);
#1932=LINE('',#10236,#2265);
#1933=LINE('',#10389,#2266);
#1934=LINE('',#10685,#2267);
#1935=LINE('',#10727,#2268);
#1936=LINE('',#10732,#2269);
#1937=LINE('',#10741,#2270);
#1938=LINE('',#10746,#2271);
#1939=LINE('',#10758,#2272);
#1940=LINE('',#10765,#2273);
#1941=LINE('',#10770,#2274);
#1942=LINE('',#10774,#2275);
#1943=LINE('',#10778,#2276);
#1944=LINE('',#10780,#2277);
#1945=LINE('',#10781,#2278);
#1946=LINE('',#10784,#2279);
#1947=LINE('',#10790,#2280);
#1948=LINE('',#10791,#2281);
#1949=LINE('',#10803,#2282);
#1950=LINE('',#10806,#2283);
#1951=LINE('',#10811,#2284);
#1952=LINE('',#10819,#2285);
#1953=LINE('',#10825,#2286);
#1954=LINE('',#10834,#2287);
#1955=LINE('',#10840,#2288);
#1956=LINE('',#10848,#2289);
#1957=LINE('',#10878,#2290);
#1958=LINE('',#10925,#2291);
#1959=LINE('',#10930,#2292);
#1960=LINE('',#10936,#2293);
#1961=LINE('',#10944,#2294);
#1962=LINE('',#10968,#2295);
#1963=LINE('',#11013,#2296);
#1964=LINE('',#11018,#2297);
#1965=LINE('',#11024,#2298);
#1966=LINE('',#11033,#2299);
#1967=LINE('',#11039,#2300);
#1968=LINE('',#11048,#2301);
#1969=LINE('',#11055,#2302);
#1970=LINE('',#11069,#2303);
#1971=LINE('',#11072,#2304);
#1972=LINE('',#11077,#2305);
#1973=LINE('',#11085,#2306);
#1974=LINE('',#11091,#2307);
#1975=LINE('',#11100,#2308);
#1976=LINE('',#11106,#2309);
#1977=LINE('',#11115,#2310);
#1978=LINE('',#11121,#2311);
#1979=LINE('',#11130,#2312);
#1980=LINE('',#11136,#2313);
#1981=LINE('',#11144,#2314);
#1982=LINE('',#11146,#2315);
#1983=LINE('',#11148,#2316);
#1984=LINE('',#11149,#2317);
#1985=LINE('',#11152,#2318);
#1986=LINE('',#11154,#2319);
#1987=LINE('',#11155,#2320);
#1988=LINE('',#11158,#2321);
#1989=LINE('',#11160,#2322);
#1990=LINE('',#11161,#2323);
#1991=LINE('',#11164,#2324);
#1992=LINE('',#11166,#2325);
#1993=LINE('',#11167,#2326);
#1994=LINE('',#11170,#2327);
#1995=LINE('',#11172,#2328);
#1996=LINE('',#11173,#2329);
#1997=LINE('',#11175,#2330);
#1998=LINE('',#11176,#2331);
#1999=LINE('',#11184,#2332);
#2000=LINE('',#11188,#2333);
#2001=LINE('',#11192,#2334);
#2002=LINE('',#11200,#2335);
#2003=LINE('',#11206,#2336);
#2004=LINE('',#11212,#2337);
#2005=LINE('',#11218,#2338);
#2006=LINE('',#11223,#2339);
#2007=LINE('',#11225,#2340);
#2008=LINE('',#11227,#2341);
#2009=LINE('',#11228,#2342);
#2010=LINE('',#11233,#2343);
#2011=LINE('',#11235,#2344);
#2012=LINE('',#11236,#2345);
#2013=LINE('',#11239,#2346);
#2014=LINE('',#11240,#2347);
#2015=LINE('',#11243,#2348);
#2016=LINE('',#11244,#2349);
#2017=LINE('',#11246,#2350);
#2018=LINE('',#11250,#2351);
#2019=LINE('',#11256,#2352);
#2020=LINE('',#11261,#2353);
#2021=LINE('',#11265,#2354);
#2022=LINE('',#11269,#2355);
#2023=LINE('',#11271,#2356);
#2024=LINE('',#11272,#2357);
#2025=LINE('',#11275,#2358);
#2026=LINE('',#11279,#2359);
#2027=LINE('',#11280,#2360);
#2028=LINE('',#11292,#2361);
#2029=LINE('',#11295,#2362);
#2030=LINE('',#11303,#2363);
#2031=LINE('',#11309,#2364);
#2032=LINE('',#11317,#2365);
#2033=LINE('',#11347,#2366);
#2034=LINE('',#11394,#2367);
#2035=LINE('',#11399,#2368);
#2036=LINE('',#11405,#2369);
#2037=LINE('',#11414,#2370);
#2038=LINE('',#11421,#2371);
#2039=LINE('',#11435,#2372);
#2040=LINE('',#11438,#2373);
#2041=LINE('',#11443,#2374);
#2042=LINE('',#11451,#2375);
#2043=LINE('',#11457,#2376);
#2044=LINE('',#11466,#2377);
#2045=LINE('',#11472,#2378);
#2046=LINE('',#11481,#2379);
#2047=LINE('',#11487,#2380);
#2048=LINE('',#11496,#2381);
#2049=LINE('',#11502,#2382);
#2050=LINE('',#11513,#2383);
#2051=LINE('',#11515,#2384);
#2052=LINE('',#11517,#2385);
#2053=LINE('',#11518,#2386);
#2054=LINE('',#11521,#2387);
#2055=LINE('',#11523,#2388);
#2056=LINE('',#11524,#2389);
#2057=LINE('',#11527,#2390);
#2058=LINE('',#11529,#2391);
#2059=LINE('',#11530,#2392);
#2060=LINE('',#11533,#2393);
#2061=LINE('',#11535,#2394);
#2062=LINE('',#11536,#2395);
#2063=LINE('',#11539,#2396);
#2064=LINE('',#11541,#2397);
#2065=LINE('',#11542,#2398);
#2066=LINE('',#11544,#2399);
#2067=LINE('',#11545,#2400);
#2068=LINE('',#11553,#2401);
#2069=LINE('',#11555,#2402);
#2070=LINE('',#11563,#2403);
#2071=LINE('',#11567,#2404);
#2072=LINE('',#11571,#2405);
#2073=LINE('',#11578,#2406);
#2074=LINE('',#11582,#2407);
#2075=LINE('',#11586,#2408);
#2076=LINE('',#11591,#2409);
#2077=LINE('',#11593,#2410);
#2078=LINE('',#11595,#2411);
#2079=LINE('',#11596,#2412);
#2080=LINE('',#11599,#2413);
#2081=LINE('',#11601,#2414);
#2082=LINE('',#11602,#2415);
#2083=LINE('',#11605,#2416);
#2084=LINE('',#11607,#2417);
#2085=LINE('',#11608,#2418);
#2086=LINE('',#11611,#2419);
#2087=LINE('',#11613,#2420);
#2088=LINE('',#11614,#2421);
#2089=LINE('',#11617,#2422);
#2090=LINE('',#11619,#2423);
#2091=LINE('',#11620,#2424);
#2092=LINE('',#11622,#2425);
#2093=LINE('',#11623,#2426);
#2094=LINE('',#11630,#2427);
#2095=LINE('',#11632,#2428);
#2096=LINE('',#11634,#2429);
#2097=LINE('',#11635,#2430);
#2098=LINE('',#11638,#2431);
#2099=LINE('',#11640,#2432);
#2100=LINE('',#11641,#2433);
#2101=LINE('',#11644,#2434);
#2102=LINE('',#11646,#2435);
#2103=LINE('',#11647,#2436);
#2104=LINE('',#11650,#2437);
#2105=LINE('',#11652,#2438);
#2106=LINE('',#11653,#2439);
#2107=LINE('',#11656,#2440);
#2108=LINE('',#11658,#2441);
#2109=LINE('',#11659,#2442);
#2110=LINE('',#11661,#2443);
#2111=LINE('',#11662,#2444);
#2112=LINE('',#11674,#2445);
#2113=LINE('',#11678,#2446);
#2114=LINE('',#11682,#2447);
#2115=LINE('',#11689,#2448);
#2116=LINE('',#11691,#2449);
#2117=LINE('',#11752,#2450);
#2118=LINE('',#11758,#2451);
#2119=LINE('',#11763,#2452);
#2120=LINE('',#11767,#2453);
#2121=LINE('',#11771,#2454);
#2122=LINE('',#11773,#2455);
#2123=LINE('',#11774,#2456);
#2124=LINE('',#11777,#2457);
#2125=LINE('',#11781,#2458);
#2126=LINE('',#11782,#2459);
#2127=LINE('',#11791,#2460);
#2128=LINE('',#11797,#2461);
#2129=LINE('',#11806,#2462);
#2130=LINE('',#11812,#2463);
#2131=VECTOR('',#7421,0.21);
#2132=VECTOR('',#7428,0.21);
#2133=VECTOR('',#7435,0.210000000000001);
#2134=VECTOR('',#7442,0.210000000000001);
#2135=VECTOR('',#7449,0.21);
#2136=VECTOR('',#7456,0.21);
#2137=VECTOR('',#7463,0.21);
#2138=VECTOR('',#7470,0.21);
#2139=VECTOR('',#7475,1.);
#2140=VECTOR('',#7476,1.);
#2141=VECTOR('',#7477,1.);
#2142=VECTOR('',#7478,1.);
#2143=VECTOR('',#7481,1.);
#2144=VECTOR('',#7482,1.);
#2145=VECTOR('',#7483,1.);
#2146=VECTOR('',#7486,1.);
#2147=VECTOR('',#7487,1.);
#2148=VECTOR('',#7488,1.);
#2149=VECTOR('',#7491,1.);
#2150=VECTOR('',#7492,1.);
#2151=VECTOR('',#7501,1.);
#2152=VECTOR('',#7502,1.);
#2153=VECTOR('',#7503,1.);
#2154=VECTOR('',#7504,1.);
#2155=VECTOR('',#7507,1.);
#2156=VECTOR('',#7508,1.);
#2157=VECTOR('',#7509,1.);
#2158=VECTOR('',#7512,1.);
#2159=VECTOR('',#7513,1.);
#2160=VECTOR('',#7514,1.);
#2161=VECTOR('',#7517,1.);
#2162=VECTOR('',#7518,1.);
#2163=VECTOR('',#7527,1.);
#2164=VECTOR('',#7528,1.);
#2165=VECTOR('',#7529,1.);
#2166=VECTOR('',#7530,1.);
#2167=VECTOR('',#7533,1.);
#2168=VECTOR('',#7534,1.);
#2169=VECTOR('',#7535,1.);
#2170=VECTOR('',#7538,1.);
#2171=VECTOR('',#7539,1.);
#2172=VECTOR('',#7540,1.);
#2173=VECTOR('',#7543,1.);
#2174=VECTOR('',#7544,1.);
#2175=VECTOR('',#7559,1.);
#2176=VECTOR('',#7562,1.);
#2177=VECTOR('',#7565,1.);
#2178=VECTOR('',#7568,1.);
#2179=VECTOR('',#7577,1.);
#2180=VECTOR('',#7580,1.);
#2181=VECTOR('',#7589,1.);
#2182=VECTOR('',#7592,1.);
#2183=VECTOR('',#7603,2.2);
#2184=VECTOR('',#7630,0.165);
#2185=VECTOR('',#7639,0.165);
#2186=VECTOR('',#7648,0.165);
#2187=VECTOR('',#7657,0.165);
#2188=VECTOR('',#7664,0.25);
#2189=VECTOR('',#7669,0.275);
#2190=VECTOR('',#7674,0.275);
#2191=VECTOR('',#7679,0.275);
#2192=VECTOR('',#7684,0.275);
#2193=VECTOR('',#7689,1.5);
#2194=VECTOR('',#7698,3.);
#2195=VECTOR('',#7703,1.02);
#2196=VECTOR('',#7716,1.02);
#2197=VECTOR('',#7723,1.49);
#2198=VECTOR('',#7736,0.225);
#2199=VECTOR('',#7743,0.225);
#2200=VECTOR('',#7750,0.225);
#2201=VECTOR('',#7757,0.225);
#2202=VECTOR('',#7764,1.49);
#2203=VECTOR('',#7775,1.02);
#2204=VECTOR('',#7780,2.2);
#2205=VECTOR('',#7797,1.);
#2206=VECTOR('',#7800,1.);
#2207=VECTOR('',#7803,1.);
#2208=VECTOR('',#7806,1.);
#2209=VECTOR('',#7815,1.);
#2210=VECTOR('',#7818,1.);
#2211=VECTOR('',#7827,1.);
#2212=VECTOR('',#7830,1.);
#2213=VECTOR('',#7841,2.2);
#2214=VECTOR('',#7868,0.165);
#2215=VECTOR('',#7877,0.165);
#2216=VECTOR('',#7886,0.164999999999999);
#2217=VECTOR('',#7895,0.164999999999999);
#2218=VECTOR('',#7902,0.25);
#2219=VECTOR('',#7907,0.275);
#2220=VECTOR('',#7912,0.275);
#2221=VECTOR('',#7917,0.275);
#2222=VECTOR('',#7922,0.275);
#2223=VECTOR('',#7927,1.5);
#2224=VECTOR('',#7936,3.);
#2225=VECTOR('',#7941,1.02);
#2226=VECTOR('',#7954,0.225);
#2227=VECTOR('',#7961,0.225);
#2228=VECTOR('',#7968,0.225);
#2229=VECTOR('',#7975,0.225);
#2230=VECTOR('',#7982,1.49);
#2231=VECTOR('',#7993,1.02);
#2232=VECTOR('',#7998,2.2);
#2233=VECTOR('',#8009,1.);
#2234=VECTOR('',#8010,1.);
#2235=VECTOR('',#8011,1.);
#2236=VECTOR('',#8012,1.);
#2237=VECTOR('',#8015,1.);
#2238=VECTOR('',#8016,1.);
#2239=VECTOR('',#8017,1.);
#2240=VECTOR('',#8020,1.);
#2241=VECTOR('',#8021,1.);
#2242=VECTOR('',#8022,1.);
#2243=VECTOR('',#8025,1.);
#2244=VECTOR('',#8026,1.);
#2245=VECTOR('',#8027,1.);
#2246=VECTOR('',#8030,1.);
#2247=VECTOR('',#8031,1.);
#2248=VECTOR('',#8032,1.);
#2249=VECTOR('',#8035,1.);
#2250=VECTOR('',#8036,1.);
#2251=VECTOR('',#8053,0.4);
#2252=VECTOR('',#8058,0.425);
#2253=VECTOR('',#8063,0.41);
#2254=VECTOR('',#8072,0.26);
#2255=VECTOR('',#8075,0.25);
#2256=VECTOR('',#8094,0.976185);
#2257=VECTOR('',#8101,0.5);
#2258=VECTOR('',#8106,0.53);
#2259=VECTOR('',#8115,0.976185);
#2260=VECTOR('',#8122,0.53);
#2261=VECTOR('',#8141,1.023815);
#2262=VECTOR('',#8152,1.47);
#2263=VECTOR('',#8157,1.5);
#2264=VECTOR('',#8162,1.47);
#2265=VECTOR('',#8167,1.023815);
#2266=VECTOR('',#8218,1.019052);
#2267=VECTOR('',#8295,0.980948);
#2268=VECTOR('',#8324,1.013815);
#2269=VECTOR('',#8331,0.991185);
#2270=VECTOR('',#8342,1.013815);
#2271=VECTOR('',#8349,0.991185);
#2272=VECTOR('',#8368,0.165);
#2273=VECTOR('',#8377,0.305);
#2274=VECTOR('',#8382,1.);
#2275=VECTOR('',#8385,1.);
#2276=VECTOR('',#8390,1.);
#2277=VECTOR('',#8391,1.);
#2278=VECTOR('',#8392,1.);
#2279=VECTOR('',#8395,1.);
#2280=VECTOR('',#8402,1.);
#2281=VECTOR('',#8403,1.);
#2282=VECTOR('',#8420,0.7);
#2283=VECTOR('',#8423,0.5);
#2284=VECTOR('',#8430,0.5);
#2285=VECTOR('',#8441,0.505);
#2286=VECTOR('',#8448,0.7);
#2287=VECTOR('',#8461,0.505);
#2288=VECTOR('',#8468,0.7);
#2289=VECTOR('',#8479,1.);
#2290=VECTOR('',#8486,0.165);
#2291=VECTOR('',#8489,1.);
#2292=VECTOR('',#8494,0.505);
#2293=VECTOR('',#8501,0.9);
#2294=VECTOR('',#8512,1.);
#2295=VECTOR('',#8519,0.165);
#2296=VECTOR('',#8522,1.);
#2297=VECTOR('',#8527,0.5);
#2298=VECTOR('',#8534,1.2);
#2299=VECTOR('',#8547,0.225);
#2300=VECTOR('',#8554,0.8);
#2301=VECTOR('',#8567,0.165);
#2302=VECTOR('',#8576,0.165);
#2303=VECTOR('',#8595,0.7);
#2304=VECTOR('',#8598,0.3);
#2305=VECTOR('',#8605,0.3);
#2306=VECTOR('',#8616,0.305);
#2307=VECTOR('',#8623,0.5);
#2308=VECTOR('',#8636,0.305);
#2309=VECTOR('',#8643,0.5);
#2310=VECTOR('',#8656,0.225);
#2311=VECTOR('',#8663,0.6);
#2312=VECTOR('',#8676,0.225);
#2313=VECTOR('',#8683,0.5);
#2314=VECTOR('',#8694,1.);
#2315=VECTOR('',#8695,1.);
#2316=VECTOR('',#8696,1.);
#2317=VECTOR('',#8697,1.);
#2318=VECTOR('',#8700,1.);
#2319=VECTOR('',#8701,1.);
#2320=VECTOR('',#8702,1.);
#2321=VECTOR('',#8705,1.);
#2322=VECTOR('',#8706,1.);
#2323=VECTOR('',#8707,1.);
#2324=VECTOR('',#8710,1.);
#2325=VECTOR('',#8711,1.);
#2326=VECTOR('',#8712,1.);
#2327=VECTOR('',#8715,1.);
#2328=VECTOR('',#8716,1.);
#2329=VECTOR('',#8717,1.);
#2330=VECTOR('',#8720,1.);
#2331=VECTOR('',#8721,1.);
#2332=VECTOR('',#8732,0.185);
#2333=VECTOR('',#8737,0.2);
#2334=VECTOR('',#8742,0.1625);
#2335=VECTOR('',#8753,0.275);
#2336=VECTOR('',#8760,0.275);
#2337=VECTOR('',#8767,0.275);
#2338=VECTOR('',#8774,0.275);
#2339=VECTOR('',#8779,1.);
#2340=VECTOR('',#8780,1.);
#2341=VECTOR('',#8781,1.);
#2342=VECTOR('',#8782,1.);
#2343=VECTOR('',#8787,1.);
#2344=VECTOR('',#8788,1.);
#2345=VECTOR('',#8789,1.);
#2346=VECTOR('',#8792,1.);
#2347=VECTOR('',#8793,1.);
#2348=VECTOR('',#8796,1.);
#2349=VECTOR('',#8797,1.);
#2350=VECTOR('',#8800,1.);
#2351=VECTOR('',#8805,0.800000000000001);
#2352=VECTOR('',#8812,0.305);
#2353=VECTOR('',#8817,1.);
#2354=VECTOR('',#8820,1.);
#2355=VECTOR('',#8825,1.);
#2356=VECTOR('',#8826,1.);
#2357=VECTOR('',#8827,1.);
#2358=VECTOR('',#8830,1.);
#2359=VECTOR('',#8835,1.);
#2360=VECTOR('',#8836,1.);
#2361=VECTOR('',#8853,0.699999999999999);
#2362=VECTOR('',#8856,0.5);
#2363=VECTOR('',#8867,0.505000000000001);
#2364=VECTOR('',#8874,0.699999999999999);
#2365=VECTOR('',#8885,1.);
#2366=VECTOR('',#8892,0.165);
#2367=VECTOR('',#8895,1.);
#2368=VECTOR('',#8900,0.505000000000001);
#2369=VECTOR('',#8907,0.9);
#2370=VECTOR('',#8920,0.164999999999999);
#2371=VECTOR('',#8929,0.164999999999999);
#2372=VECTOR('',#8948,0.699999999999999);
#2373=VECTOR('',#8951,0.300000000000001);
#2374=VECTOR('',#8958,0.300000000000001);
#2375=VECTOR('',#8969,0.305);
#2376=VECTOR('',#8976,0.5);
#2377=VECTOR('',#8989,0.305);
#2378=VECTOR('',#8996,0.5);
#2379=VECTOR('',#9009,0.225);
#2380=VECTOR('',#9016,0.6);
#2381=VECTOR('',#9029,0.225);
#2382=VECTOR('',#9036,0.5);
#2383=VECTOR('',#9051,1.);
#2384=VECTOR('',#9052,1.);
#2385=VECTOR('',#9053,1.);
#2386=VECTOR('',#9054,1.);
#2387=VECTOR('',#9057,1.);
#2388=VECTOR('',#9058,1.);
#2389=VECTOR('',#9059,1.);
#2390=VECTOR('',#9062,1.);
#2391=VECTOR('',#9063,1.);
#2392=VECTOR('',#9064,1.);
#2393=VECTOR('',#9067,1.);
#2394=VECTOR('',#9068,1.);
#2395=VECTOR('',#9069,1.);
#2396=VECTOR('',#9072,1.);
#2397=VECTOR('',#9073,1.);
#2398=VECTOR('',#9074,1.);
#2399=VECTOR('',#9077,1.);
#2400=VECTOR('',#9078,1.);
#2401=VECTOR('',#9089,0.185);
#2402=VECTOR('',#9092,0.2);
#2403=VECTOR('',#9103,0.325);
#2404=VECTOR('',#9108,0.35);
#2405=VECTOR('',#9113,0.335);
#2406=VECTOR('',#9122,0.21);
#2407=VECTOR('',#9127,0.2);
#2408=VECTOR('',#9132,0.18);
#2409=VECTOR('',#9137,1.);
#2410=VECTOR('',#9138,1.);
#2411=VECTOR('',#9139,1.);
#2412=VECTOR('',#9140,1.);
#2413=VECTOR('',#9143,1.);
#2414=VECTOR('',#9144,1.);
#2415=VECTOR('',#9145,1.);
#2416=VECTOR('',#9148,1.);
#2417=VECTOR('',#9149,1.);
#2418=VECTOR('',#9150,1.);
#2419=VECTOR('',#9153,1.);
#2420=VECTOR('',#9154,1.);
#2421=VECTOR('',#9155,1.);
#2422=VECTOR('',#9158,1.);
#2423=VECTOR('',#9159,1.);
#2424=VECTOR('',#9160,1.);
#2425=VECTOR('',#9163,1.);
#2426=VECTOR('',#9164,1.);
#2427=VECTOR('',#9173,1.);
#2428=VECTOR('',#9174,1.);
#2429=VECTOR('',#9175,1.);
#2430=VECTOR('',#9176,1.);
#2431=VECTOR('',#9179,1.);
#2432=VECTOR('',#9180,1.);
#2433=VECTOR('',#9181,1.);
#2434=VECTOR('',#9184,1.);
#2435=VECTOR('',#9185,1.);
#2436=VECTOR('',#9186,1.);
#2437=VECTOR('',#9189,1.);
#2438=VECTOR('',#9190,1.);
#2439=VECTOR('',#9191,1.);
#2440=VECTOR('',#9194,1.);
#2441=VECTOR('',#9195,1.);
#2442=VECTOR('',#9196,1.);
#2443=VECTOR('',#9199,1.);
#2444=VECTOR('',#9200,1.);
#2445=VECTOR('',#9217,0.325);
#2446=VECTOR('',#9222,0.35);
#2447=VECTOR('',#9227,0.335);
#2448=VECTOR('',#9236,0.21);
#2449=VECTOR('',#9239,0.2);
#2450=VECTOR('',#9356,0.5);
#2451=VECTOR('',#9363,0.5);
#2452=VECTOR('',#9368,1.);
#2453=VECTOR('',#9371,1.);
#2454=VECTOR('',#9376,1.);
#2455=VECTOR('',#9377,1.);
#2456=VECTOR('',#9378,1.);
#2457=VECTOR('',#9381,1.);
#2458=VECTOR('',#9386,1.);
#2459=VECTOR('',#9387,1.);
#2460=VECTOR('',#9400,0.305);
#2461=VECTOR('',#9407,0.5);
#2462=VECTOR('',#9420,0.305);
#2463=VECTOR('',#9427,0.5);
#2464=CIRCLE('',#6563,0.21);
#2465=CIRCLE('',#6564,0.21);
#2466=CIRCLE('',#6566,0.21);
#2467=CIRCLE('',#6567,0.21);
#2468=CIRCLE('',#6569,0.210000000000001);
#2469=CIRCLE('',#6570,0.210000000000001);
#2470=CIRCLE('',#6572,0.210000000000001);
#2471=CIRCLE('',#6573,0.210000000000001);
#2472=CIRCLE('',#6575,0.21);
#2473=CIRCLE('',#6576,0.21);
#2474=CIRCLE('',#6578,0.21);
#2475=CIRCLE('',#6579,0.21);
#2476=CIRCLE('',#6581,0.21);
#2477=CIRCLE('',#6582,0.21);
#2478=CIRCLE('',#6584,0.21);
#2479=CIRCLE('',#6585,0.21);
#2480=CIRCLE('',#6608,2.2);
#2481=CIRCLE('',#6609,0.525);
#2482=CIRCLE('',#6611,0.525);
#2483=CIRCLE('',#6613,0.525);
#2484=CIRCLE('',#6614,0.525);
#2485=CIRCLE('',#6616,2.2);
#2486=CIRCLE('',#6618,0.525);
#2487=CIRCLE('',#6619,0.525);
#2488=CIRCLE('',#6621,2.2);
#2489=CIRCLE('',#6623,0.525);
#2490=CIRCLE('',#6624,0.525);
#2491=CIRCLE('',#6626,2.2);
#2492=CIRCLE('',#6628,2.2);
#2493=CIRCLE('',#6629,2.2);
#2494=CIRCLE('',#6630,2.2);
#2495=CIRCLE('',#6631,2.2);
#2496=CIRCLE('',#6632,2.2);
#2497=CIRCLE('',#6633,2.2);
#2498=CIRCLE('',#6635,3.);
#2499=CIRCLE('',#6636,0.275);
#2500=CIRCLE('',#6637,0.275);
#2501=CIRCLE('',#6638,0.275);
#2502=CIRCLE('',#6639,0.275);
#2503=CIRCLE('',#6641,0.165);
#2504=CIRCLE('',#6642,0.165);
#2505=CIRCLE('',#6645,0.165);
#2506=CIRCLE('',#6646,0.165);
#2507=CIRCLE('',#6649,0.165);
#2508=CIRCLE('',#6650,0.165);
#2509=CIRCLE('',#6653,0.165);
#2510=CIRCLE('',#6654,0.165);
#2511=CIRCLE('',#6658,0.275);
#2512=CIRCLE('',#6660,0.275);
#2513=CIRCLE('',#6662,0.275);
#2514=CIRCLE('',#6664,0.275);
#2515=CIRCLE('',#6666,1.5);
#2516=CIRCLE('',#6667,1.5);
#2517=CIRCLE('',#6669,1.02);
#2518=CIRCLE('',#6671,3.);
#2519=CIRCLE('',#6673,1.02);
#2520=CIRCLE('',#6678,1.02);
#2521=CIRCLE('',#6679,1.02);
#2522=CIRCLE('',#6681,1.49);
#2523=CIRCLE('',#6682,1.49);
#2524=CIRCLE('',#6687,0.225);
#2525=CIRCLE('',#6688,0.225);
#2526=CIRCLE('',#6690,0.225);
#2527=CIRCLE('',#6691,0.225);
#2528=CIRCLE('',#6693,0.225);
#2529=CIRCLE('',#6694,0.225);
#2530=CIRCLE('',#6696,0.225);
#2531=CIRCLE('',#6697,0.225);
#2532=CIRCLE('',#6699,1.49);
#2533=CIRCLE('',#6700,1.49);
#2534=CIRCLE('',#6702,1.02);
#2535=CIRCLE('',#6704,1.02);
#2536=CIRCLE('',#6706,2.2);
#2537=CIRCLE('',#6707,2.2);
#2538=CIRCLE('',#6712,2.2);
#2539=CIRCLE('',#6713,0.525);
#2540=CIRCLE('',#6715,0.525);
#2541=CIRCLE('',#6717,0.525);
#2542=CIRCLE('',#6718,0.525);
#2543=CIRCLE('',#6720,2.2);
#2544=CIRCLE('',#6722,0.525);
#2545=CIRCLE('',#6723,0.525);
#2546=CIRCLE('',#6725,2.2);
#2547=CIRCLE('',#6727,0.525);
#2548=CIRCLE('',#6728,0.525);
#2549=CIRCLE('',#6730,2.2);
#2550=CIRCLE('',#6732,2.2);
#2551=CIRCLE('',#6733,2.2);
#2552=CIRCLE('',#6734,2.2);
#2553=CIRCLE('',#6735,2.2);
#2554=CIRCLE('',#6736,2.2);
#2555=CIRCLE('',#6737,2.2);
#2556=CIRCLE('',#6739,3.);
#2557=CIRCLE('',#6740,0.275);
#2558=CIRCLE('',#6741,0.275);
#2559=CIRCLE('',#6742,0.275);
#2560=CIRCLE('',#6743,0.275);
#2561=CIRCLE('',#6745,0.165);
#2562=CIRCLE('',#6746,0.165);
#2563=CIRCLE('',#6749,0.165);
#2564=CIRCLE('',#6750,0.165);
#2565=CIRCLE('',#6753,0.164999999999999);
#2566=CIRCLE('',#6754,0.164999999999999);
#2567=CIRCLE('',#6757,0.164999999999999);
#2568=CIRCLE('',#6758,0.164999999999999);
#2569=CIRCLE('',#6762,0.275);
#2570=CIRCLE('',#6764,0.275);
#2571=CIRCLE('',#6766,0.275);
#2572=CIRCLE('',#6768,0.275);
#2573=CIRCLE('',#6770,1.5);
#2574=CIRCLE('',#6771,1.5);
#2575=CIRCLE('',#6773,1.02);
#2576=CIRCLE('',#6775,3.);
#2577=CIRCLE('',#6777,1.02);
#2578=CIRCLE('',#6782,0.225);
#2579=CIRCLE('',#6783,0.225);
#2580=CIRCLE('',#6785,0.225);
#2581=CIRCLE('',#6786,0.225);
#2582=CIRCLE('',#6788,0.225);
#2583=CIRCLE('',#6789,0.225);
#2584=CIRCLE('',#6791,0.225);
#2585=CIRCLE('',#6792,0.225);
#2586=CIRCLE('',#6794,1.49);
#2587=CIRCLE('',#6795,1.49);
#2588=CIRCLE('',#6797,1.02);
#2589=CIRCLE('',#6799,1.02);
#2590=CIRCLE('',#6801,2.2);
#2591=CIRCLE('',#6802,2.2);
#2592=CIRCLE('',#6815,0.24505);
#2593=CIRCLE('',#6817,0.375);
#2594=CIRCLE('',#6819,0.425);
#2595=CIRCLE('',#6821,0.425);
#2596=CIRCLE('',#6823,0.395);
#2597=CIRCLE('',#6825,0.27);
#2598=CIRCLE('',#6827,0.24505);
#2599=CIRCLE('',#6832,0.976185);
#2600=CIRCLE('',#6833,0.976185);
#2601=CIRCLE('',#6834,0.247676);
#2602=CIRCLE('',#6835,0.976185);
#2603=CIRCLE('',#6836,0.976185);
#2604=CIRCLE('',#6838,0.976185);
#2605=CIRCLE('',#6840,0.5);
#2606=CIRCLE('',#6841,0.5);
#2607=CIRCLE('',#6843,0.56);
#2608=CIRCLE('',#6846,0.976185);
#2609=CIRCLE('',#6848,0.56);
#2610=CIRCLE('',#6852,1.023815);
#2611=CIRCLE('',#6853,1.023815);
#2612=CIRCLE('',#6854,0.247676);
#2613=CIRCLE('',#6855,1.023815);
#2614=CIRCLE('',#6856,1.023815);
#2615=CIRCLE('',#6858,1.023815);
#2616=CIRCLE('',#6860,1.44);
#2617=CIRCLE('',#6861,1.023815);
#2618=CIRCLE('',#6863,1.5);
#2619=CIRCLE('',#6865,1.5);
#2620=CIRCLE('',#6867,1.44);
#2621=CIRCLE('',#6872,0.23815);
#2622=CIRCLE('',#6874,0.23815);
#2623=CIRCLE('',#6876,0.23815);
#2624=CIRCLE('',#6878,0.23815);
#2625=CIRCLE('',#6880,0.23815);
#2626=CIRCLE('',#6882,0.23815);
#2627=CIRCLE('',#6884,0.23815);
#2628=CIRCLE('',#6886,0.23815);
#2629=CIRCLE('',#6889,0.243053047864041);
#2630=CIRCLE('',#6890,0.243053047864041);
#2631=CIRCLE('',#6892,1.019052);
#2632=CIRCLE('',#6893,1.019052);
#2633=CIRCLE('',#6894,1.019052);
#2634=CIRCLE('',#6895,1.019052);
#2635=CIRCLE('',#6896,1.019052);
#2636=CIRCLE('',#6897,1.019052);
#2637=CIRCLE('',#6898,1.019052);
#2638=CIRCLE('',#6899,1.019052);
#2639=CIRCLE('',#6900,1.019052);
#2640=CIRCLE('',#6902,0.980948);
#2641=CIRCLE('',#6903,0.243053047864041);
#2642=CIRCLE('',#6905,0.243053047864041);
#2643=CIRCLE('',#6907,0.980948);
#2644=CIRCLE('',#6908,0.243053047864041);
#2645=CIRCLE('',#6910,0.243053047864041);
#2646=CIRCLE('',#6912,0.980948);
#2647=CIRCLE('',#6913,0.243053047864041);
#2648=CIRCLE('',#6915,0.243053047864041);
#2649=CIRCLE('',#6917,0.980948);
#2650=CIRCLE('',#6918,0.243053047864041);
#2651=CIRCLE('',#6920,0.243053047864041);
#2652=CIRCLE('',#6922,0.980948);
#2653=CIRCLE('',#6923,0.243053047864041);
#2654=CIRCLE('',#6925,0.243053047864041);
#2655=CIRCLE('',#6927,0.980948);
#2656=CIRCLE('',#6928,0.243053047864041);
#2657=CIRCLE('',#6930,0.243053047864041);
#2658=CIRCLE('',#6932,0.980948);
#2659=CIRCLE('',#6933,0.980948);
#2660=CIRCLE('',#6934,0.980948);
#2661=CIRCLE('',#6936,0.243053047864041);
#2662=CIRCLE('',#6938,0.243053047864041);
#2663=CIRCLE('',#6943,1.013815);
#2664=CIRCLE('',#6944,0.991185);
#2665=CIRCLE('',#6946,1.013815);
#2666=CIRCLE('',#6948,0.991185);
#2667=CIRCLE('',#6951,1.013815);
#2668=CIRCLE('',#6952,0.991185);
#2669=CIRCLE('',#6954,1.013815);
#2670=CIRCLE('',#6956,0.991185);
#2671=CIRCLE('',#6966,0.165);
#2672=CIRCLE('',#6967,0.165);
#2673=CIRCLE('',#6970,0.305);
#2674=CIRCLE('',#6971,0.305);
#2675=CIRCLE('',#6973,0.7);
#2676=CIRCLE('',#6974,0.7);
#2677=CIRCLE('',#6977,1.);
#2678=CIRCLE('',#6978,0.5);
#2679=CIRCLE('',#6981,1.);
#2680=CIRCLE('',#6983,0.7);
#2681=CIRCLE('',#6985,0.7);
#2682=CIRCLE('',#6986,0.5);
#2683=CIRCLE('',#6989,0.5);
#2684=CIRCLE('',#6991,0.5);
#2685=CIRCLE('',#6996,0.505);
#2686=CIRCLE('',#6997,0.505);
#2687=CIRCLE('',#6999,0.7);
#2688=CIRCLE('',#7000,0.7);
#2689=CIRCLE('',#7005,0.505);
#2690=CIRCLE('',#7006,0.505);
#2691=CIRCLE('',#7008,0.7);
#2692=CIRCLE('',#7009,0.7);
#2693=CIRCLE('',#7014,0.165);
#2694=CIRCLE('',#7016,0.165);
#2695=CIRCLE('',#7019,0.505);
#2696=CIRCLE('',#7020,0.505);
#2697=CIRCLE('',#7022,0.9);
#2698=CIRCLE('',#7023,0.9);
#2699=CIRCLE('',#7028,0.165);
#2700=CIRCLE('',#7030,0.165);
#2701=CIRCLE('',#7033,0.5);
#2702=CIRCLE('',#7034,0.5);
#2703=CIRCLE('',#7036,1.2);
#2704=CIRCLE('',#7037,1.2);
#2705=CIRCLE('',#7042,0.225);
#2706=CIRCLE('',#7043,0.225);
#2707=CIRCLE('',#7045,0.8);
#2708=CIRCLE('',#7046,0.8);
#2709=CIRCLE('',#7051,0.165);
#2710=CIRCLE('',#7052,0.165);
#2711=CIRCLE('',#7055,0.165);
#2712=CIRCLE('',#7056,0.165);
#2713=CIRCLE('',#7059,0.7);
#2714=CIRCLE('',#7060,0.3);
#2715=CIRCLE('',#7062,0.7);
#2716=CIRCLE('',#7063,0.3);
#2717=CIRCLE('',#7066,0.3);
#2718=CIRCLE('',#7068,0.3);
#2719=CIRCLE('',#7073,0.305);
#2720=CIRCLE('',#7074,0.305);
#2721=CIRCLE('',#7076,0.5);
#2722=CIRCLE('',#7077,0.5);
#2723=CIRCLE('',#7082,0.305);
#2724=CIRCLE('',#7083,0.305);
#2725=CIRCLE('',#7085,0.5);
#2726=CIRCLE('',#7086,0.5);
#2727=CIRCLE('',#7091,0.225);
#2728=CIRCLE('',#7092,0.225);
#2729=CIRCLE('',#7094,0.6);
#2730=CIRCLE('',#7095,0.6);
#2731=CIRCLE('',#7100,0.225);
#2732=CIRCLE('',#7101,0.225);
#2733=CIRCLE('',#7103,0.5);
#2734=CIRCLE('',#7104,0.5);
#2735=CIRCLE('',#7116,0.17);
#2736=CIRCLE('',#7118,0.1954);
#2737=CIRCLE('',#7120,0.1954);
#2738=CIRCLE('',#7122,0.125);
#2739=CIRCLE('',#7127,0.275);
#2740=CIRCLE('',#7128,0.275);
#2741=CIRCLE('',#7130,0.275);
#2742=CIRCLE('',#7131,0.275);
#2743=CIRCLE('',#7133,0.275);
#2744=CIRCLE('',#7134,0.275);
#2745=CIRCLE('',#7136,0.275);
#2746=CIRCLE('',#7137,0.275);
#2747=CIRCLE('',#7139,0.800000000000001);
#2748=CIRCLE('',#7146,0.800000000000001);
#2749=CIRCLE('',#7148,0.305);
#2750=CIRCLE('',#7149,0.305);
#2751=CIRCLE('',#7151,0.699999999999999);
#2752=CIRCLE('',#7152,0.699999999999999);
#2753=CIRCLE('',#7155,1.);
#2754=CIRCLE('',#7158,1.);
#2755=CIRCLE('',#7160,0.699999999999999);
#2756=CIRCLE('',#7162,0.699999999999999);
#2757=CIRCLE('',#7163,0.5);
#2758=CIRCLE('',#7166,0.5);
#2759=CIRCLE('',#7170,0.505000000000001);
#2760=CIRCLE('',#7171,0.505000000000001);
#2761=CIRCLE('',#7173,0.699999999999999);
#2762=CIRCLE('',#7174,0.699999999999999);
#2763=CIRCLE('',#7179,0.165);
#2764=CIRCLE('',#7181,0.165);
#2765=CIRCLE('',#7184,0.505000000000001);
#2766=CIRCLE('',#7185,0.505000000000001);
#2767=CIRCLE('',#7187,0.9);
#2768=CIRCLE('',#7188,0.9);
#2769=CIRCLE('',#7193,0.164999999999999);
#2770=CIRCLE('',#7194,0.164999999999999);
#2771=CIRCLE('',#7197,0.164999999999999);
#2772=CIRCLE('',#7198,0.164999999999999);
#2773=CIRCLE('',#7201,0.699999999999999);
#2774=CIRCLE('',#7202,0.300000000000001);
#2775=CIRCLE('',#7204,0.699999999999999);
#2776=CIRCLE('',#7205,0.300000000000001);
#2777=CIRCLE('',#7208,0.300000000000001);
#2778=CIRCLE('',#7210,0.300000000000001);
#2779=CIRCLE('',#7215,0.305);
#2780=CIRCLE('',#7216,0.305);
#2781=CIRCLE('',#7218,0.5);
#2782=CIRCLE('',#7219,0.5);
#2783=CIRCLE('',#7224,0.305);
#2784=CIRCLE('',#7225,0.305);
#2785=CIRCLE('',#7227,0.5);
#2786=CIRCLE('',#7228,0.5);
#2787=CIRCLE('',#7233,0.225);
#2788=CIRCLE('',#7234,0.225);
#2789=CIRCLE('',#7236,0.6);
#2790=CIRCLE('',#7237,0.6);
#2791=CIRCLE('',#7242,0.225);
#2792=CIRCLE('',#7243,0.225);
#2793=CIRCLE('',#7245,0.5);
#2794=CIRCLE('',#7246,0.5);
#2795=CIRCLE('',#7251,0.1954);
#2796=CIRCLE('',#7260,0.17);
#2797=CIRCLE('',#7262,0.1954);
#2798=CIRCLE('',#7266,0.3);
#2799=CIRCLE('',#7268,0.35);
#2800=CIRCLE('',#7270,0.35);
#2801=CIRCLE('',#7272,0.32);
#2802=CIRCLE('',#7274,0.22);
#2803=CIRCLE('',#7276,0.1954);
#2804=CIRCLE('',#7278,0.1954);
#2805=CIRCLE('',#7280,0.16);
#2806=CIRCLE('',#7300,0.1954);
#2807=CIRCLE('',#7302,0.3);
#2808=CIRCLE('',#7304,0.35);
#2809=CIRCLE('',#7306,0.35);
#2810=CIRCLE('',#7308,0.32);
#2811=CIRCLE('',#7310,0.22);
#2812=CIRCLE('',#7312,0.1954);
#2813=CIRCLE('',#7371,0.5);
#2814=CIRCLE('',#7372,0.5);
#2815=CIRCLE('',#7374,0.5);
#2816=CIRCLE('',#7375,0.5);
#2817=CIRCLE('',#7377,1.);
#2818=CIRCLE('',#7378,1.);
#2819=CIRCLE('',#7381,1.);
#2820=CIRCLE('',#7384,1.);
#2821=CIRCLE('',#7388,0.305);
#2822=CIRCLE('',#7389,0.305);
#2823=CIRCLE('',#7391,0.5);
#2824=CIRCLE('',#7392,0.5);
#2825=CIRCLE('',#7397,0.305);
#2826=CIRCLE('',#7398,0.305);
#2827=CIRCLE('',#7400,0.5);
#2828=CIRCLE('',#7401,0.5);
#2829=VERTEX_POINT('',#9452);
#2830=VERTEX_POINT('',#9454);
#2831=VERTEX_POINT('',#9458);
#2832=VERTEX_POINT('',#9460);
#2833=VERTEX_POINT('',#9464);
#2834=VERTEX_POINT('',#9466);
#2835=VERTEX_POINT('',#9470);
#2836=VERTEX_POINT('',#9472);
#2837=VERTEX_POINT('',#9476);
#2838=VERTEX_POINT('',#9478);
#2839=VERTEX_POINT('',#9482);
#2840=VERTEX_POINT('',#9484);
#2841=VERTEX_POINT('',#9488);
#2842=VERTEX_POINT('',#9490);
#2843=VERTEX_POINT('',#9494);
#2844=VERTEX_POINT('',#9496);
#2845=VERTEX_POINT('',#9500);
#2846=VERTEX_POINT('',#9501);
#2847=VERTEX_POINT('',#9503);
#2848=VERTEX_POINT('',#9505);
#2849=VERTEX_POINT('',#9509);
#2850=VERTEX_POINT('',#9511);
#2851=VERTEX_POINT('',#9515);
#2852=VERTEX_POINT('',#9517);
#2853=VERTEX_POINT('',#9527);
#2854=VERTEX_POINT('',#9528);
#2855=VERTEX_POINT('',#9530);
#2856=VERTEX_POINT('',#9532);
#2857=VERTEX_POINT('',#9536);
#2858=VERTEX_POINT('',#9538);
#2859=VERTEX_POINT('',#9542);
#2860=VERTEX_POINT('',#9544);
#2861=VERTEX_POINT('',#9554);
#2862=VERTEX_POINT('',#9555);
#2863=VERTEX_POINT('',#9557);
#2864=VERTEX_POINT('',#9559);
#2865=VERTEX_POINT('',#9563);
#2866=VERTEX_POINT('',#9565);
#2867=VERTEX_POINT('',#9569);
#2868=VERTEX_POINT('',#9571);
#2869=VERTEX_POINT('',#9581);
#2870=VERTEX_POINT('',#9582);
#2871=VERTEX_POINT('',#9586);
#2872=VERTEX_POINT('',#9588);
#2873=VERTEX_POINT('',#9592);
#2874=VERTEX_POINT('',#9593);
#2875=VERTEX_POINT('',#9595);
#2876=VERTEX_POINT('',#9597);
#2877=VERTEX_POINT('',#9603);
#2878=VERTEX_POINT('',#9604);
#2879=VERTEX_POINT('',#9606);
#2880=VERTEX_POINT('',#9608);
#2881=VERTEX_POINT('',#9614);
#2882=VERTEX_POINT('',#9615);
#2883=VERTEX_POINT('',#9617);
#2884=VERTEX_POINT('',#9619);
#2885=VERTEX_POINT('',#9625);
#2886=VERTEX_POINT('',#9627);
#2887=VERTEX_POINT('',#9635);
#2888=VERTEX_POINT('',#9637);
#2889=VERTEX_POINT('',#9639);
#2890=VERTEX_POINT('',#9641);
#2891=VERTEX_POINT('',#9643);
#2892=VERTEX_POINT('',#9646);
#2893=VERTEX_POINT('',#9648);
#2894=VERTEX_POINT('',#9653);
#2895=VERTEX_POINT('',#9655);
#2896=VERTEX_POINT('',#9660);
#2897=VERTEX_POINT('',#9662);
#2898=VERTEX_POINT('',#9667);
#2899=VERTEX_POINT('',#9669);
#2900=VERTEX_POINT('',#9674);
#2901=VERTEX_POINT('',#9675);
#2902=VERTEX_POINT('',#9712);
#2903=VERTEX_POINT('',#9714);
#2904=VERTEX_POINT('',#9752);
#2905=VERTEX_POINT('',#9756);
#2906=VERTEX_POINT('',#9760);
#2907=VERTEX_POINT('',#9764);
#2908=VERTEX_POINT('',#9768);
#2909=VERTEX_POINT('',#9770);
#2910=VERTEX_POINT('',#9774);
#2911=VERTEX_POINT('',#9777);
#2912=VERTEX_POINT('',#9781);
#2913=VERTEX_POINT('',#9788);
#2914=VERTEX_POINT('',#9790);
#2915=VERTEX_POINT('',#9794);
#2916=VERTEX_POINT('',#9796);
#2917=VERTEX_POINT('',#9803);
#2918=VERTEX_POINT('',#9805);
#2919=VERTEX_POINT('',#9809);
#2920=VERTEX_POINT('',#9811);
#2921=VERTEX_POINT('',#9815);
#2922=VERTEX_POINT('',#9817);
#2923=VERTEX_POINT('',#9821);
#2924=VERTEX_POINT('',#9823);
#2925=VERTEX_POINT('',#9827);
#2926=VERTEX_POINT('',#9829);
#2927=VERTEX_POINT('',#9833);
#2928=VERTEX_POINT('',#9836);
#2929=VERTEX_POINT('',#9840);
#2930=VERTEX_POINT('',#9842);
#2931=VERTEX_POINT('',#9849);
#2932=VERTEX_POINT('',#9850);
#2933=VERTEX_POINT('',#9854);
#2934=VERTEX_POINT('',#9856);
#2935=VERTEX_POINT('',#9860);
#2936=VERTEX_POINT('',#9861);
#2937=VERTEX_POINT('',#9863);
#2938=VERTEX_POINT('',#9865);
#2939=VERTEX_POINT('',#9871);
#2940=VERTEX_POINT('',#9872);
#2941=VERTEX_POINT('',#9874);
#2942=VERTEX_POINT('',#9876);
#2943=VERTEX_POINT('',#9882);
#2944=VERTEX_POINT('',#9883);
#2945=VERTEX_POINT('',#9885);
#2946=VERTEX_POINT('',#9887);
#2947=VERTEX_POINT('',#9893);
#2948=VERTEX_POINT('',#9895);
#2949=VERTEX_POINT('',#9903);
#2950=VERTEX_POINT('',#9905);
#2951=VERTEX_POINT('',#9907);
#2952=VERTEX_POINT('',#9909);
#2953=VERTEX_POINT('',#9911);
#2954=VERTEX_POINT('',#9914);
#2955=VERTEX_POINT('',#9916);
#2956=VERTEX_POINT('',#9921);
#2957=VERTEX_POINT('',#9923);
#2958=VERTEX_POINT('',#9928);
#2959=VERTEX_POINT('',#9930);
#2960=VERTEX_POINT('',#9935);
#2961=VERTEX_POINT('',#9937);
#2962=VERTEX_POINT('',#9942);
#2963=VERTEX_POINT('',#9943);
#2964=VERTEX_POINT('',#9980);
#2965=VERTEX_POINT('',#9982);
#2966=VERTEX_POINT('',#10020);
#2967=VERTEX_POINT('',#10024);
#2968=VERTEX_POINT('',#10028);
#2969=VERTEX_POINT('',#10032);
#2970=VERTEX_POINT('',#10036);
#2971=VERTEX_POINT('',#10038);
#2972=VERTEX_POINT('',#10042);
#2973=VERTEX_POINT('',#10045);
#2974=VERTEX_POINT('',#10049);
#2975=VERTEX_POINT('',#10056);
#2976=VERTEX_POINT('',#10058);
#2977=VERTEX_POINT('',#10062);
#2978=VERTEX_POINT('',#10064);
#2979=VERTEX_POINT('',#10068);
#2980=VERTEX_POINT('',#10070);
#2981=VERTEX_POINT('',#10074);
#2982=VERTEX_POINT('',#10076);
#2983=VERTEX_POINT('',#10080);
#2984=VERTEX_POINT('',#10082);
#2985=VERTEX_POINT('',#10086);
#2986=VERTEX_POINT('',#10089);
#2987=VERTEX_POINT('',#10093);
#2988=VERTEX_POINT('',#10095);
#2989=VERTEX_POINT('',#10102);
#2990=VERTEX_POINT('',#10103);
#2991=VERTEX_POINT('',#10105);
#2992=VERTEX_POINT('',#10107);
#2993=VERTEX_POINT('',#10111);
#2994=VERTEX_POINT('',#10113);
#2995=VERTEX_POINT('',#10117);
#2996=VERTEX_POINT('',#10119);
#2997=VERTEX_POINT('',#10123);
#2998=VERTEX_POINT('',#10125);
#2999=VERTEX_POINT('',#10129);
#3000=VERTEX_POINT('',#10131);
#3001=VERTEX_POINT('',#10140);
#3002=VERTEX_POINT('',#10143);
#3003=VERTEX_POINT('',#10146);
#3004=VERTEX_POINT('',#10150);
#3005=VERTEX_POINT('',#10154);
#3006=VERTEX_POINT('',#10158);
#3007=VERTEX_POINT('',#10161);
#3008=VERTEX_POINT('',#10169);
#3009=VERTEX_POINT('',#10170);
#3010=VERTEX_POINT('',#10173);
#3011=VERTEX_POINT('',#10175);
#3012=VERTEX_POINT('',#10179);
#3013=VERTEX_POINT('',#10183);
#3014=VERTEX_POINT('',#10185);
#3015=VERTEX_POINT('',#10189);
#3016=VERTEX_POINT('',#10194);
#3017=VERTEX_POINT('',#10198);
#3018=VERTEX_POINT('',#10204);
#3019=VERTEX_POINT('',#10205);
#3020=VERTEX_POINT('',#10208);
#3021=VERTEX_POINT('',#10210);
#3022=VERTEX_POINT('',#10214);
#3023=VERTEX_POINT('',#10218);
#3024=VERTEX_POINT('',#10220);
#3025=VERTEX_POINT('',#10223);
#3026=VERTEX_POINT('',#10227);
#3027=VERTEX_POINT('',#10231);
#3028=VERTEX_POINT('',#10239);
#3029=VERTEX_POINT('',#10240);
#3030=VERTEX_POINT('',#10243);
#3031=VERTEX_POINT('',#10244);
#3032=VERTEX_POINT('',#10247);
#3033=VERTEX_POINT('',#10248);
#3034=VERTEX_POINT('',#10251);
#3035=VERTEX_POINT('',#10252);
#3036=VERTEX_POINT('',#10255);
#3037=VERTEX_POINT('',#10256);
#3038=VERTEX_POINT('',#10259);
#3039=VERTEX_POINT('',#10260);
#3040=VERTEX_POINT('',#10263);
#3041=VERTEX_POINT('',#10264);
#3042=VERTEX_POINT('',#10267);
#3043=VERTEX_POINT('',#10268);
#3044=VERTEX_POINT('',#10272);
#3045=VERTEX_POINT('',#10273);
#3046=VERTEX_POINT('',#10296);
#3047=VERTEX_POINT('',#10298);
#3048=VERTEX_POINT('',#10323);
#3049=VERTEX_POINT('',#10325);
#3050=VERTEX_POINT('',#10348);
#3051=VERTEX_POINT('',#10350);
#3052=VERTEX_POINT('',#10373);
#3053=VERTEX_POINT('',#10375);
#3054=VERTEX_POINT('',#10388);
#3055=VERTEX_POINT('',#10391);
#3056=VERTEX_POINT('',#10404);
#3057=VERTEX_POINT('',#10406);
#3058=VERTEX_POINT('',#10429);
#3059=VERTEX_POINT('',#10431);
#3060=VERTEX_POINT('',#10454);
#3061=VERTEX_POINT('',#10456);
#3062=VERTEX_POINT('',#10479);
#3063=VERTEX_POINT('',#10481);
#3064=VERTEX_POINT('',#10506);
#3065=VERTEX_POINT('',#10510);
#3066=VERTEX_POINT('',#10535);
#3067=VERTEX_POINT('',#10539);
#3068=VERTEX_POINT('',#10564);
#3069=VERTEX_POINT('',#10568);
#3070=VERTEX_POINT('',#10569);
#3071=VERTEX_POINT('',#10596);
#3072=VERTEX_POINT('',#10600);
#3073=VERTEX_POINT('',#10625);
#3074=VERTEX_POINT('',#10629);
#3075=VERTEX_POINT('',#10654);
#3076=VERTEX_POINT('',#10658);
#3077=VERTEX_POINT('',#10683);
#3078=VERTEX_POINT('',#10686);
#3079=VERTEX_POINT('',#10688);
#3080=VERTEX_POINT('',#10720);
#3081=VERTEX_POINT('',#10722);
#3082=VERTEX_POINT('',#10725);
#3083=VERTEX_POINT('',#10729);
#3084=VERTEX_POINT('',#10734);
#3085=VERTEX_POINT('',#10736);
#3086=VERTEX_POINT('',#10739);
#3087=VERTEX_POINT('',#10743);
#3088=VERTEX_POINT('',#10755);
#3089=VERTEX_POINT('',#10757);
#3090=VERTEX_POINT('',#10762);
#3091=VERTEX_POINT('',#10764);
#3092=VERTEX_POINT('',#10768);
#3093=VERTEX_POINT('',#10769);
#3094=VERTEX_POINT('',#10771);
#3095=VERTEX_POINT('',#10773);
#3096=VERTEX_POINT('',#10777);
#3097=VERTEX_POINT('',#10779);
#3098=VERTEX_POINT('',#10783);
#3099=VERTEX_POINT('',#10786);
#3100=VERTEX_POINT('',#10789);
#3101=VERTEX_POINT('',#10795);
#3102=VERTEX_POINT('',#10798);
#3103=VERTEX_POINT('',#10800);
#3104=VERTEX_POINT('',#10805);
#3105=VERTEX_POINT('',#10809);
#3106=VERTEX_POINT('',#10816);
#3107=VERTEX_POINT('',#10818);
#3108=VERTEX_POINT('',#10822);
#3109=VERTEX_POINT('',#10824);
#3110=VERTEX_POINT('',#10831);
#3111=VERTEX_POINT('',#10833);
#3112=VERTEX_POINT('',#10837);
#3113=VERTEX_POINT('',#10839);
#3114=VERTEX_POINT('',#10846);
#3115=VERTEX_POINT('',#10847);
#3116=VERTEX_POINT('',#10851);
#3117=VERTEX_POINT('',#10866);
#3118=VERTEX_POINT('',#10868);
#3119=VERTEX_POINT('',#10877);
#3120=VERTEX_POINT('',#10879);
#3121=VERTEX_POINT('',#10927);
#3122=VERTEX_POINT('',#10929);
#3123=VERTEX_POINT('',#10933);
#3124=VERTEX_POINT('',#10935);
#3125=VERTEX_POINT('',#10942);
#3126=VERTEX_POINT('',#10943);
#3127=VERTEX_POINT('',#10947);
#3128=VERTEX_POINT('',#10958);
#3129=VERTEX_POINT('',#10960);
#3130=VERTEX_POINT('',#10967);
#3131=VERTEX_POINT('',#10969);
#3132=VERTEX_POINT('',#11015);
#3133=VERTEX_POINT('',#11017);
#3134=VERTEX_POINT('',#11021);
#3135=VERTEX_POINT('',#11023);
#3136=VERTEX_POINT('',#11030);
#3137=VERTEX_POINT('',#11032);
#3138=VERTEX_POINT('',#11036);
#3139=VERTEX_POINT('',#11038);
#3140=VERTEX_POINT('',#11045);
#3141=VERTEX_POINT('',#11047);
#3142=VERTEX_POINT('',#11052);
#3143=VERTEX_POINT('',#11054);
#3144=VERTEX_POINT('',#11059);
#3145=VERTEX_POINT('',#11061);
#3146=VERTEX_POINT('',#11064);
#3147=VERTEX_POINT('',#11066);
#3148=VERTEX_POINT('',#11071);
#3149=VERTEX_POINT('',#11075);
#3150=VERTEX_POINT('',#11082);
#3151=VERTEX_POINT('',#11084);
#3152=VERTEX_POINT('',#11088);
#3153=VERTEX_POINT('',#11090);
#3154=VERTEX_POINT('',#11097);
#3155=VERTEX_POINT('',#11099);
#3156=VERTEX_POINT('',#11103);
#3157=VERTEX_POINT('',#11105);
#3158=VERTEX_POINT('',#11112);
#3159=VERTEX_POINT('',#11114);
#3160=VERTEX_POINT('',#11118);
#3161=VERTEX_POINT('',#11120);
#3162=VERTEX_POINT('',#11127);
#3163=VERTEX_POINT('',#11129);
#3164=VERTEX_POINT('',#11133);
#3165=VERTEX_POINT('',#11135);
#3166=VERTEX_POINT('',#11142);
#3167=VERTEX_POINT('',#11143);
#3168=VERTEX_POINT('',#11145);
#3169=VERTEX_POINT('',#11147);
#3170=VERTEX_POINT('',#11151);
#3171=VERTEX_POINT('',#11153);
#3172=VERTEX_POINT('',#11157);
#3173=VERTEX_POINT('',#11159);
#3174=VERTEX_POINT('',#11163);
#3175=VERTEX_POINT('',#11165);
#3176=VERTEX_POINT('',#11169);
#3177=VERTEX_POINT('',#11171);
#3178=VERTEX_POINT('',#11179);
#3179=VERTEX_POINT('',#11182);
#3180=VERTEX_POINT('',#11186);
#3181=VERTEX_POINT('',#11190);
#3182=VERTEX_POINT('',#11197);
#3183=VERTEX_POINT('',#11199);
#3184=VERTEX_POINT('',#11203);
#3185=VERTEX_POINT('',#11205);
#3186=VERTEX_POINT('',#11209);
#3187=VERTEX_POINT('',#11211);
#3188=VERTEX_POINT('',#11215);
#3189=VERTEX_POINT('',#11217);
#3190=VERTEX_POINT('',#11221);
#3191=VERTEX_POINT('',#11222);
#3192=VERTEX_POINT('',#11224);
#3193=VERTEX_POINT('',#11226);
#3194=VERTEX_POINT('',#11229);
#3195=VERTEX_POINT('',#11232);
#3196=VERTEX_POINT('',#11234);
#3197=VERTEX_POINT('',#11238);
#3198=VERTEX_POINT('',#11242);
#3199=VERTEX_POINT('',#11249);
#3200=VERTEX_POINT('',#11253);
#3201=VERTEX_POINT('',#11255);
#3202=VERTEX_POINT('',#11259);
#3203=VERTEX_POINT('',#11260);
#3204=VERTEX_POINT('',#11262);
#3205=VERTEX_POINT('',#11264);
#3206=VERTEX_POINT('',#11268);
#3207=VERTEX_POINT('',#11270);
#3208=VERTEX_POINT('',#11274);
#3209=VERTEX_POINT('',#11278);
#3210=VERTEX_POINT('',#11284);
#3211=VERTEX_POINT('',#11287);
#3212=VERTEX_POINT('',#11289);
#3213=VERTEX_POINT('',#11294);
#3214=VERTEX_POINT('',#11300);
#3215=VERTEX_POINT('',#11302);
#3216=VERTEX_POINT('',#11306);
#3217=VERTEX_POINT('',#11308);
#3218=VERTEX_POINT('',#11315);
#3219=VERTEX_POINT('',#11316);
#3220=VERTEX_POINT('',#11320);
#3221=VERTEX_POINT('',#11335);
#3222=VERTEX_POINT('',#11337);
#3223=VERTEX_POINT('',#11346);
#3224=VERTEX_POINT('',#11348);
#3225=VERTEX_POINT('',#11396);
#3226=VERTEX_POINT('',#11398);
#3227=VERTEX_POINT('',#11402);
#3228=VERTEX_POINT('',#11404);
#3229=VERTEX_POINT('',#11411);
#3230=VERTEX_POINT('',#11413);
#3231=VERTEX_POINT('',#11418);
#3232=VERTEX_POINT('',#11420);
#3233=VERTEX_POINT('',#11425);
#3234=VERTEX_POINT('',#11427);
#3235=VERTEX_POINT('',#11430);
#3236=VERTEX_POINT('',#11432);
#3237=VERTEX_POINT('',#11437);
#3238=VERTEX_POINT('',#11441);
#3239=VERTEX_POINT('',#11448);
#3240=VERTEX_POINT('',#11450);
#3241=VERTEX_POINT('',#11454);
#3242=VERTEX_POINT('',#11456);
#3243=VERTEX_POINT('',#11463);
#3244=VERTEX_POINT('',#11465);
#3245=VERTEX_POINT('',#11469);
#3246=VERTEX_POINT('',#11471);
#3247=VERTEX_POINT('',#11478);
#3248=VERTEX_POINT('',#11480);
#3249=VERTEX_POINT('',#11484);
#3250=VERTEX_POINT('',#11486);
#3251=VERTEX_POINT('',#11493);
#3252=VERTEX_POINT('',#11495);
#3253=VERTEX_POINT('',#11499);
#3254=VERTEX_POINT('',#11501);
#3255=VERTEX_POINT('',#11508);
#3256=VERTEX_POINT('',#11511);
#3257=VERTEX_POINT('',#11512);
#3258=VERTEX_POINT('',#11514);
#3259=VERTEX_POINT('',#11516);
#3260=VERTEX_POINT('',#11520);
#3261=VERTEX_POINT('',#11522);
#3262=VERTEX_POINT('',#11526);
#3263=VERTEX_POINT('',#11528);
#3264=VERTEX_POINT('',#11532);
#3265=VERTEX_POINT('',#11534);
#3266=VERTEX_POINT('',#11538);
#3267=VERTEX_POINT('',#11540);
#3268=VERTEX_POINT('',#11548);
#3269=VERTEX_POINT('',#11551);
#3270=VERTEX_POINT('',#11558);
#3271=VERTEX_POINT('',#11561);
#3272=VERTEX_POINT('',#11565);
#3273=VERTEX_POINT('',#11569);
#3274=VERTEX_POINT('',#11573);
#3275=VERTEX_POINT('',#11576);
#3276=VERTEX_POINT('',#11580);
#3277=VERTEX_POINT('',#11584);
#3278=VERTEX_POINT('',#11589);
#3279=VERTEX_POINT('',#11590);
#3280=VERTEX_POINT('',#11592);
#3281=VERTEX_POINT('',#11594);
#3282=VERTEX_POINT('',#11598);
#3283=VERTEX_POINT('',#11600);
#3284=VERTEX_POINT('',#11604);
#3285=VERTEX_POINT('',#11606);
#3286=VERTEX_POINT('',#11610);
#3287=VERTEX_POINT('',#11612);
#3288=VERTEX_POINT('',#11616);
#3289=VERTEX_POINT('',#11618);
#3290=VERTEX_POINT('',#11628);
#3291=VERTEX_POINT('',#11629);
#3292=VERTEX_POINT('',#11631);
#3293=VERTEX_POINT('',#11633);
#3294=VERTEX_POINT('',#11637);
#3295=VERTEX_POINT('',#11639);
#3296=VERTEX_POINT('',#11643);
#3297=VERTEX_POINT('',#11645);
#3298=VERTEX_POINT('',#11649);
#3299=VERTEX_POINT('',#11651);
#3300=VERTEX_POINT('',#11655);
#3301=VERTEX_POINT('',#11657);
#3302=VERTEX_POINT('',#11666);
#3303=VERTEX_POINT('',#11669);
#3304=VERTEX_POINT('',#11672);
#3305=VERTEX_POINT('',#11676);
#3306=VERTEX_POINT('',#11680);
#3307=VERTEX_POINT('',#11684);
#3308=VERTEX_POINT('',#11687);
#3309=VERTEX_POINT('',#11749);
#3310=VERTEX_POINT('',#11751);
#3311=VERTEX_POINT('',#11755);
#3312=VERTEX_POINT('',#11757);
#3313=VERTEX_POINT('',#11761);
#3314=VERTEX_POINT('',#11762);
#3315=VERTEX_POINT('',#11764);
#3316=VERTEX_POINT('',#11766);
#3317=VERTEX_POINT('',#11770);
#3318=VERTEX_POINT('',#11772);
#3319=VERTEX_POINT('',#11776);
#3320=VERTEX_POINT('',#11780);
#3321=VERTEX_POINT('',#11788);
#3322=VERTEX_POINT('',#11790);
#3323=VERTEX_POINT('',#11794);
#3324=VERTEX_POINT('',#11796);
#3325=VERTEX_POINT('',#11803);
#3326=VERTEX_POINT('',#11805);
#3327=VERTEX_POINT('',#11809);
#3328=VERTEX_POINT('',#11811);
#3329=EDGE_CURVE('',#2829,#2829,#2464,.T.);
#3330=EDGE_CURVE('',#2829,#2830,#1798,.T.);
#3331=EDGE_CURVE('',#2830,#2830,#2465,.T.);
#3332=EDGE_CURVE('',#2831,#2831,#2466,.T.);
#3333=EDGE_CURVE('',#2831,#2832,#1799,.T.);
#3334=EDGE_CURVE('',#2832,#2832,#2467,.T.);
#3335=EDGE_CURVE('',#2833,#2833,#2468,.T.);
#3336=EDGE_CURVE('',#2833,#2834,#1800,.T.);
#3337=EDGE_CURVE('',#2834,#2834,#2469,.T.);
#3338=EDGE_CURVE('',#2835,#2835,#2470,.T.);
#3339=EDGE_CURVE('',#2835,#2836,#1801,.T.);
#3340=EDGE_CURVE('',#2836,#2836,#2471,.T.);
#3341=EDGE_CURVE('',#2837,#2837,#2472,.T.);
#3342=EDGE_CURVE('',#2837,#2838,#1802,.T.);
#3343=EDGE_CURVE('',#2838,#2838,#2473,.T.);
#3344=EDGE_CURVE('',#2839,#2839,#2474,.T.);
#3345=EDGE_CURVE('',#2839,#2840,#1803,.T.);
#3346=EDGE_CURVE('',#2840,#2840,#2475,.T.);
#3347=EDGE_CURVE('',#2841,#2841,#2476,.T.);
#3348=EDGE_CURVE('',#2841,#2842,#1804,.T.);
#3349=EDGE_CURVE('',#2842,#2842,#2477,.T.);
#3350=EDGE_CURVE('',#2843,#2843,#2478,.T.);
#3351=EDGE_CURVE('',#2843,#2844,#1805,.T.);
#3352=EDGE_CURVE('',#2844,#2844,#2479,.T.);
#3353=EDGE_CURVE('',#2845,#2846,#1806,.T.);
#3354=EDGE_CURVE('',#2846,#2847,#1807,.T.);
#3355=EDGE_CURVE('',#2848,#2847,#1808,.T.);
#3356=EDGE_CURVE('',#2845,#2848,#1809,.T.);
#3357=EDGE_CURVE('',#2849,#2845,#1810,.T.);
#3358=EDGE_CURVE('',#2850,#2848,#1811,.T.);
#3359=EDGE_CURVE('',#2849,#2850,#1812,.T.);
#3360=EDGE_CURVE('',#2851,#2849,#1813,.T.);
#3361=EDGE_CURVE('',#2852,#2850,#1814,.T.);
#3362=EDGE_CURVE('',#2851,#2852,#1815,.T.);
#3363=EDGE_CURVE('',#2846,#2851,#1816,.T.);
#3364=EDGE_CURVE('',#2847,#2852,#1817,.T.);
#3365=EDGE_CURVE('',#2853,#2854,#1818,.T.);
#3366=EDGE_CURVE('',#2854,#2855,#1819,.T.);
#3367=EDGE_CURVE('',#2856,#2855,#1820,.T.);
#3368=EDGE_CURVE('',#2853,#2856,#1821,.T.);
#3369=EDGE_CURVE('',#2857,#2853,#1822,.T.);
#3370=EDGE_CURVE('',#2858,#2856,#1823,.T.);
#3371=EDGE_CURVE('',#2857,#2858,#1824,.T.);
#3372=EDGE_CURVE('',#2859,#2857,#1825,.T.);
#3373=EDGE_CURVE('',#2860,#2858,#1826,.T.);
#3374=EDGE_CURVE('',#2859,#2860,#1827,.T.);
#3375=EDGE_CURVE('',#2854,#2859,#1828,.T.);
#3376=EDGE_CURVE('',#2855,#2860,#1829,.T.);
#3377=EDGE_CURVE('',#2861,#2862,#1830,.T.);
#3378=EDGE_CURVE('',#2862,#2863,#1831,.T.);
#3379=EDGE_CURVE('',#2864,#2863,#1832,.T.);
#3380=EDGE_CURVE('',#2861,#2864,#1833,.T.);
#3381=EDGE_CURVE('',#2865,#2861,#1834,.T.);
#3382=EDGE_CURVE('',#2866,#2864,#1835,.T.);
#3383=EDGE_CURVE('',#2865,#2866,#1836,.T.);
#3384=EDGE_CURVE('',#2867,#2865,#1837,.T.);
#3385=EDGE_CURVE('',#2868,#2866,#1838,.T.);
#3386=EDGE_CURVE('',#2867,#2868,#1839,.T.);
#3387=EDGE_CURVE('',#2862,#2867,#1840,.T.);
#3388=EDGE_CURVE('',#2863,#2868,#1841,.T.);
#3389=EDGE_CURVE('',#2869,#2870,#2480,.T.);
#3390=EDGE_CURVE('',#2870,#2869,#2481,.T.);
#3391=EDGE_CURVE('',#2871,#2869,#1842,.T.);
#3392=EDGE_CURVE('',#2872,#2871,#2482,.T.);
#3393=EDGE_CURVE('',#2870,#2872,#1843,.T.);
#3394=EDGE_CURVE('',#2873,#2874,#1844,.T.);
#3395=EDGE_CURVE('',#2873,#2875,#2483,.T.);
#3396=EDGE_CURVE('',#2876,#2875,#1845,.T.);
#3397=EDGE_CURVE('',#2874,#2876,#2484,.T.);
#3398=EDGE_CURVE('',#2875,#2873,#2485,.T.);
#3399=EDGE_CURVE('',#2877,#2878,#1846,.T.);
#3400=EDGE_CURVE('',#2877,#2879,#2486,.T.);
#3401=EDGE_CURVE('',#2880,#2879,#1847,.T.);
#3402=EDGE_CURVE('',#2878,#2880,#2487,.T.);
#3403=EDGE_CURVE('',#2879,#2877,#2488,.T.);
#3404=EDGE_CURVE('',#2881,#2882,#1848,.T.);
#3405=EDGE_CURVE('',#2881,#2883,#2489,.T.);
#3406=EDGE_CURVE('',#2884,#2883,#1849,.T.);
#3407=EDGE_CURVE('',#2882,#2884,#2490,.T.);
#3408=EDGE_CURVE('',#2883,#2881,#2491,.T.);
#3409=EDGE_CURVE('',#2885,#2885,#2492,.T.);
#3410=EDGE_CURVE('',#2885,#2886,#1850,.T.);
#3411=EDGE_CURVE('',#2886,#2871,#2493,.T.);
#3412=EDGE_CURVE('',#2872,#2884,#2494,.T.);
#3413=EDGE_CURVE('',#2882,#2880,#2495,.T.);
#3414=EDGE_CURVE('',#2878,#2876,#2496,.T.);
#3415=EDGE_CURVE('',#2874,#2886,#2497,.T.);
#3416=EDGE_CURVE('',#2887,#2887,#2498,.T.);
#3417=EDGE_CURVE('',#2888,#2888,#2499,.T.);
#3418=EDGE_CURVE('',#2889,#2889,#2500,.T.);
#3419=EDGE_CURVE('',#2890,#2890,#2501,.T.);
#3420=EDGE_CURVE('',#2891,#2891,#2502,.T.);
#3421=EDGE_CURVE('',#2892,#2892,#2503,.T.);
#3422=EDGE_CURVE('',#2892,#2893,#1851,.T.);
#3423=EDGE_CURVE('',#2893,#2893,#2504,.T.);
#3424=EDGE_CURVE('',#2894,#2894,#2505,.T.);
#3425=EDGE_CURVE('',#2894,#2895,#1852,.T.);
#3426=EDGE_CURVE('',#2895,#2895,#2506,.T.);
#3427=EDGE_CURVE('',#2896,#2896,#2507,.T.);
#3428=EDGE_CURVE('',#2896,#2897,#1853,.T.);
#3429=EDGE_CURVE('',#2897,#2897,#2508,.T.);
#3430=EDGE_CURVE('',#2898,#2898,#2509,.T.);
#3431=EDGE_CURVE('',#2898,#2899,#1854,.T.);
#3432=EDGE_CURVE('',#2899,#2899,#2510,.T.);
#3433=EDGE_CURVE('',#2900,#2901,#316,.T.);
#3434=EDGE_CURVE('',#2901,#2900,#317,.T.);
#3435=EDGE_CURVE('',#2901,#2902,#1855,.T.);
#3436=EDGE_CURVE('',#2903,#2902,#318,.T.);
#3437=EDGE_CURVE('',#2902,#2903,#319,.T.);
#3438=EDGE_CURVE('',#2904,#2904,#2511,.T.);
#3439=EDGE_CURVE('',#2904,#2888,#1856,.T.);
#3440=EDGE_CURVE('',#2905,#2905,#2512,.T.);
#3441=EDGE_CURVE('',#2905,#2891,#1857,.T.);
#3442=EDGE_CURVE('',#2906,#2906,#2513,.T.);
#3443=EDGE_CURVE('',#2906,#2889,#1858,.T.);
#3444=EDGE_CURVE('',#2907,#2907,#2514,.T.);
#3445=EDGE_CURVE('',#2907,#2890,#1859,.T.);
#3446=EDGE_CURVE('',#2908,#2908,#2515,.T.);
#3447=EDGE_CURVE('',#2908,#2909,#1860,.T.);
#3448=EDGE_CURVE('',#2909,#2909,#2516,.T.);
#3449=EDGE_CURVE('',#2910,#2910,#2517,.T.);
#3450=EDGE_CURVE('',#2887,#2911,#1861,.T.);
#3451=EDGE_CURVE('',#2911,#2911,#2518,.T.);
#3452=EDGE_CURVE('',#2910,#2912,#1862,.T.);
#3453=EDGE_CURVE('',#2912,#2912,#2519,.T.);
#3454=EDGE_CURVE('',#2913,#2913,#2520,.T.);
#3455=EDGE_CURVE('',#2913,#2914,#1863,.T.);
#3456=EDGE_CURVE('',#2914,#2914,#2521,.T.);
#3457=EDGE_CURVE('',#2915,#2915,#2522,.T.);
#3458=EDGE_CURVE('',#2915,#2916,#1864,.T.);
#3459=EDGE_CURVE('',#2916,#2916,#2523,.T.);
#3460=EDGE_CURVE('',#2917,#2917,#2524,.T.);
#3461=EDGE_CURVE('',#2917,#2918,#1865,.T.);
#3462=EDGE_CURVE('',#2918,#2918,#2525,.T.);
#3463=EDGE_CURVE('',#2919,#2919,#2526,.T.);
#3464=EDGE_CURVE('',#2919,#2920,#1866,.T.);
#3465=EDGE_CURVE('',#2920,#2920,#2527,.T.);
#3466=EDGE_CURVE('',#2921,#2921,#2528,.T.);
#3467=EDGE_CURVE('',#2921,#2922,#1867,.T.);
#3468=EDGE_CURVE('',#2922,#2922,#2529,.T.);
#3469=EDGE_CURVE('',#2923,#2923,#2530,.T.);
#3470=EDGE_CURVE('',#2923,#2924,#1868,.T.);
#3471=EDGE_CURVE('',#2924,#2924,#2531,.T.);
#3472=EDGE_CURVE('',#2925,#2925,#2532,.T.);
#3473=EDGE_CURVE('',#2925,#2926,#1869,.T.);
#3474=EDGE_CURVE('',#2926,#2926,#2533,.T.);
#3475=EDGE_CURVE('',#2927,#2927,#2534,.T.);
#3476=EDGE_CURVE('',#2928,#2928,#2535,.T.);
#3477=EDGE_CURVE('',#2928,#2927,#1870,.T.);
#3478=EDGE_CURVE('',#2929,#2929,#2536,.T.);
#3479=EDGE_CURVE('',#2929,#2930,#1871,.T.);
#3480=EDGE_CURVE('',#2930,#2930,#2537,.T.);
#3481=EDGE_CURVE('',#2931,#2932,#2538,.T.);
#3482=EDGE_CURVE('',#2932,#2931,#2539,.T.);
#3483=EDGE_CURVE('',#2933,#2931,#1872,.T.);
#3484=EDGE_CURVE('',#2934,#2933,#2540,.T.);
#3485=EDGE_CURVE('',#2932,#2934,#1873,.T.);
#3486=EDGE_CURVE('',#2935,#2936,#1874,.T.);
#3487=EDGE_CURVE('',#2935,#2937,#2541,.T.);
#3488=EDGE_CURVE('',#2938,#2937,#1875,.T.);
#3489=EDGE_CURVE('',#2936,#2938,#2542,.T.);
#3490=EDGE_CURVE('',#2937,#2935,#2543,.T.);
#3491=EDGE_CURVE('',#2939,#2940,#1876,.T.);
#3492=EDGE_CURVE('',#2939,#2941,#2544,.T.);
#3493=EDGE_CURVE('',#2942,#2941,#1877,.T.);
#3494=EDGE_CURVE('',#2940,#2942,#2545,.T.);
#3495=EDGE_CURVE('',#2941,#2939,#2546,.T.);
#3496=EDGE_CURVE('',#2943,#2944,#1878,.T.);
#3497=EDGE_CURVE('',#2943,#2945,#2547,.T.);
#3498=EDGE_CURVE('',#2946,#2945,#1879,.T.);
#3499=EDGE_CURVE('',#2944,#2946,#2548,.T.);
#3500=EDGE_CURVE('',#2945,#2943,#2549,.T.);
#3501=EDGE_CURVE('',#2947,#2947,#2550,.T.);
#3502=EDGE_CURVE('',#2947,#2948,#1880,.T.);
#3503=EDGE_CURVE('',#2948,#2933,#2551,.T.);
#3504=EDGE_CURVE('',#2934,#2946,#2552,.T.);
#3505=EDGE_CURVE('',#2944,#2942,#2553,.T.);
#3506=EDGE_CURVE('',#2940,#2938,#2554,.T.);
#3507=EDGE_CURVE('',#2936,#2948,#2555,.T.);
#3508=EDGE_CURVE('',#2949,#2949,#2556,.T.);
#3509=EDGE_CURVE('',#2950,#2950,#2557,.T.);
#3510=EDGE_CURVE('',#2951,#2951,#2558,.T.);
#3511=EDGE_CURVE('',#2952,#2952,#2559,.T.);
#3512=EDGE_CURVE('',#2953,#2953,#2560,.T.);
#3513=EDGE_CURVE('',#2954,#2954,#2561,.T.);
#3514=EDGE_CURVE('',#2954,#2955,#1881,.T.);
#3515=EDGE_CURVE('',#2955,#2955,#2562,.T.);
#3516=EDGE_CURVE('',#2956,#2956,#2563,.T.);
#3517=EDGE_CURVE('',#2956,#2957,#1882,.T.);
#3518=EDGE_CURVE('',#2957,#2957,#2564,.T.);
#3519=EDGE_CURVE('',#2958,#2958,#2565,.T.);
#3520=EDGE_CURVE('',#2958,#2959,#1883,.T.);
#3521=EDGE_CURVE('',#2959,#2959,#2566,.T.);
#3522=EDGE_CURVE('',#2960,#2960,#2567,.T.);
#3523=EDGE_CURVE('',#2960,#2961,#1884,.T.);
#3524=EDGE_CURVE('',#2961,#2961,#2568,.T.);
#3525=EDGE_CURVE('',#2962,#2963,#320,.T.);
#3526=EDGE_CURVE('',#2963,#2962,#321,.T.);
#3527=EDGE_CURVE('',#2963,#2964,#1885,.T.);
#3528=EDGE_CURVE('',#2965,#2964,#322,.T.);
#3529=EDGE_CURVE('',#2964,#2965,#323,.T.);
#3530=EDGE_CURVE('',#2966,#2966,#2569,.T.);
#3531=EDGE_CURVE('',#2966,#2950,#1886,.T.);
#3532=EDGE_CURVE('',#2967,#2967,#2570,.T.);
#3533=EDGE_CURVE('',#2967,#2953,#1887,.T.);
#3534=EDGE_CURVE('',#2968,#2968,#2571,.T.);
#3535=EDGE_CURVE('',#2968,#2951,#1888,.T.);
#3536=EDGE_CURVE('',#2969,#2969,#2572,.T.);
#3537=EDGE_CURVE('',#2969,#2952,#1889,.T.);
#3538=EDGE_CURVE('',#2970,#2970,#2573,.T.);
#3539=EDGE_CURVE('',#2970,#2971,#1890,.T.);
#3540=EDGE_CURVE('',#2971,#2971,#2574,.T.);
#3541=EDGE_CURVE('',#2972,#2972,#2575,.T.);
#3542=EDGE_CURVE('',#2949,#2973,#1891,.T.);
#3543=EDGE_CURVE('',#2973,#2973,#2576,.T.);
#3544=EDGE_CURVE('',#2972,#2974,#1892,.T.);
#3545=EDGE_CURVE('',#2974,#2974,#2577,.T.);
#3546=EDGE_CURVE('',#2975,#2975,#2578,.T.);
#3547=EDGE_CURVE('',#2975,#2976,#1893,.T.);
#3548=EDGE_CURVE('',#2976,#2976,#2579,.T.);
#3549=EDGE_CURVE('',#2977,#2977,#2580,.T.);
#3550=EDGE_CURVE('',#2977,#2978,#1894,.T.);
#3551=EDGE_CURVE('',#2978,#2978,#2581,.T.);
#3552=EDGE_CURVE('',#2979,#2979,#2582,.T.);
#3553=EDGE_CURVE('',#2979,#2980,#1895,.T.);
#3554=EDGE_CURVE('',#2980,#2980,#2583,.T.);
#3555=EDGE_CURVE('',#2981,#2981,#2584,.T.);
#3556=EDGE_CURVE('',#2981,#2982,#1896,.T.);
#3557=EDGE_CURVE('',#2982,#2982,#2585,.T.);
#3558=EDGE_CURVE('',#2983,#2983,#2586,.T.);
#3559=EDGE_CURVE('',#2983,#2984,#1897,.T.);
#3560=EDGE_CURVE('',#2984,#2984,#2587,.T.);
#3561=EDGE_CURVE('',#2985,#2985,#2588,.T.);
#3562=EDGE_CURVE('',#2986,#2986,#2589,.T.);
#3563=EDGE_CURVE('',#2986,#2985,#1898,.T.);
#3564=EDGE_CURVE('',#2987,#2987,#2590,.T.);
#3565=EDGE_CURVE('',#2987,#2988,#1899,.T.);
#3566=EDGE_CURVE('',#2988,#2988,#2591,.T.);
#3567=EDGE_CURVE('',#2989,#2990,#1900,.T.);
#3568=EDGE_CURVE('',#2990,#2991,#1901,.T.);
#3569=EDGE_CURVE('',#2991,#2992,#1902,.T.);
#3570=EDGE_CURVE('',#2989,#2992,#1903,.T.);
#3571=EDGE_CURVE('',#2990,#2993,#1904,.T.);
#3572=EDGE_CURVE('',#2993,#2994,#1905,.T.);
#3573=EDGE_CURVE('',#2994,#2991,#1906,.T.);
#3574=EDGE_CURVE('',#2993,#2995,#1907,.T.);
#3575=EDGE_CURVE('',#2995,#2996,#1908,.T.);
#3576=EDGE_CURVE('',#2996,#2994,#1909,.T.);
#3577=EDGE_CURVE('',#2995,#2997,#1910,.T.);
#3578=EDGE_CURVE('',#2997,#2998,#1911,.T.);
#3579=EDGE_CURVE('',#2998,#2996,#1912,.T.);
#3580=EDGE_CURVE('',#2997,#2999,#1913,.T.);
#3581=EDGE_CURVE('',#2999,#3000,#1914,.T.);
#3582=EDGE_CURVE('',#3000,#2998,#1915,.T.);
#3583=EDGE_CURVE('',#2999,#2989,#1916,.T.);
#3584=EDGE_CURVE('',#2992,#3000,#1917,.T.);
#3585=EDGE_CURVE('',#3001,#3001,#2592,.T.);
#3586=EDGE_CURVE('',#3002,#3002,#2593,.T.);
#3587=EDGE_CURVE('',#3003,#3003,#2594,.T.);
#3588=EDGE_CURVE('',#3003,#3002,#1918,.T.);
#3589=EDGE_CURVE('',#3004,#3004,#2595,.T.);
#3590=EDGE_CURVE('',#3004,#3003,#1919,.T.);
#3591=EDGE_CURVE('',#3005,#3005,#2596,.T.);
#3592=EDGE_CURVE('',#3005,#3004,#1920,.T.);
#3593=EDGE_CURVE('',#3006,#3006,#2597,.T.);
#3594=EDGE_CURVE('',#3007,#3007,#2598,.F.);
#3595=EDGE_CURVE('',#3007,#3006,#1921,.T.);
#3596=EDGE_CURVE('',#3001,#3007,#1922,.T.);
#3597=EDGE_CURVE('',#3008,#3009,#2599,.T.);
#3598=EDGE_CURVE('',#3009,#3008,#2600,.T.);
#3599=EDGE_CURVE('',#3009,#3010,#2601,.T.);
#3600=EDGE_CURVE('',#3011,#3010,#2602,.T.);
#3601=EDGE_CURVE('',#3010,#3011,#2603,.T.);
#3602=EDGE_CURVE('',#3011,#3012,#1923,.T.);
#3603=EDGE_CURVE('',#3012,#3012,#2604,.T.);
#3604=EDGE_CURVE('',#3013,#3013,#2605,.T.);
#3605=EDGE_CURVE('',#3013,#3014,#1924,.T.);
#3606=EDGE_CURVE('',#3014,#3014,#2606,.T.);
#3607=EDGE_CURVE('',#3014,#3015,#1925,.T.);
#3608=EDGE_CURVE('',#3015,#3015,#2607,.T.);
#3609=EDGE_CURVE('',#3016,#3016,#2608,.T.);
#3610=EDGE_CURVE('',#3016,#3008,#1926,.T.);
#3611=EDGE_CURVE('',#3017,#3017,#2609,.T.);
#3612=EDGE_CURVE('',#3017,#3013,#1927,.T.);
#3613=EDGE_CURVE('',#3018,#3019,#2610,.T.);
#3614=EDGE_CURVE('',#3019,#3018,#2611,.T.);
#3615=EDGE_CURVE('',#3019,#3020,#2612,.T.);
#3616=EDGE_CURVE('',#3021,#3020,#2613,.T.);
#3617=EDGE_CURVE('',#3020,#3021,#2614,.T.);
#3618=EDGE_CURVE('',#3022,#3022,#2615,.T.);
#3619=EDGE_CURVE('',#3022,#3021,#1928,.T.);
#3620=EDGE_CURVE('',#3023,#3023,#2616,.T.);
#3621=EDGE_CURVE('',#3024,#3024,#2617,.T.);
#3622=EDGE_CURVE('',#3025,#3025,#2618,.T.);
#3623=EDGE_CURVE('',#3025,#3023,#1929,.T.);
#3624=EDGE_CURVE('',#3026,#3026,#2619,.T.);
#3625=EDGE_CURVE('',#3026,#3025,#1930,.T.);
#3626=EDGE_CURVE('',#3027,#3027,#2620,.T.);
#3627=EDGE_CURVE('',#3027,#3026,#1931,.T.);
#3628=EDGE_CURVE('',#3018,#3024,#1932,.T.);
#3629=EDGE_CURVE('',#3028,#3029,#2621,.T.);
#3630=EDGE_CURVE('',#3030,#3031,#2622,.T.);
#3631=EDGE_CURVE('',#3032,#3033,#2623,.T.);
#3632=EDGE_CURVE('',#3034,#3035,#2624,.T.);
#3633=EDGE_CURVE('',#3036,#3037,#2625,.T.);
#3634=EDGE_CURVE('',#3038,#3039,#2626,.T.);
#3635=EDGE_CURVE('',#3040,#3041,#2627,.T.);
#3636=EDGE_CURVE('',#3042,#3043,#2628,.T.);
#3637=EDGE_CURVE('',#3044,#3045,#324,.T.);
#3638=EDGE_CURVE('',#3046,#3044,#2629,.T.);
#3639=EDGE_CURVE('',#3047,#3046,#325,.T.);
#3640=EDGE_CURVE('',#3045,#3047,#2630,.T.);
#3641=EDGE_CURVE('',#3048,#3046,#2631,.T.);
#3642=EDGE_CURVE('',#3048,#3049,#326,.T.);
#3643=EDGE_CURVE('',#3050,#3049,#2632,.T.);
#3644=EDGE_CURVE('',#3050,#3051,#327,.T.);
#3645=EDGE_CURVE('',#3052,#3051,#2633,.T.);
#3646=EDGE_CURVE('',#3052,#3053,#328,.T.);
#3647=EDGE_CURVE('',#3053,#3054,#1933,.T.);
#3648=EDGE_CURVE('',#3054,#3054,#2634,.T.);
#3649=EDGE_CURVE('',#3053,#3055,#329,.T.);
#3650=EDGE_CURVE('',#3056,#3055,#2635,.T.);
#3651=EDGE_CURVE('',#3056,#3057,#330,.T.);
#3652=EDGE_CURVE('',#3058,#3057,#2636,.T.);
#3653=EDGE_CURVE('',#3058,#3059,#331,.T.);
#3654=EDGE_CURVE('',#3060,#3059,#2637,.T.);
#3655=EDGE_CURVE('',#3060,#3061,#332,.T.);
#3656=EDGE_CURVE('',#3062,#3061,#2638,.T.);
#3657=EDGE_CURVE('',#3062,#3063,#333,.T.);
#3658=EDGE_CURVE('',#3047,#3063,#2639,.T.);
#3659=EDGE_CURVE('',#3044,#3064,#2640,.T.);
#3660=EDGE_CURVE('',#3064,#3048,#2641,.T.);
#3661=EDGE_CURVE('',#3065,#3064,#334,.T.);
#3662=EDGE_CURVE('',#3049,#3065,#2642,.T.);
#3663=EDGE_CURVE('',#3065,#3066,#2643,.T.);
#3664=EDGE_CURVE('',#3066,#3050,#2644,.T.);
#3665=EDGE_CURVE('',#3067,#3066,#335,.T.);
#3666=EDGE_CURVE('',#3051,#3067,#2645,.T.);
#3667=EDGE_CURVE('',#3067,#3068,#2646,.T.);
#3668=EDGE_CURVE('',#3068,#3052,#2647,.T.);
#3669=EDGE_CURVE('',#3069,#3070,#336,.T.);
#3670=EDGE_CURVE('',#3055,#3069,#2648,.T.);
#3671=EDGE_CURVE('',#3070,#3068,#337,.T.);
#3672=EDGE_CURVE('',#3069,#3071,#2649,.T.);
#3673=EDGE_CURVE('',#3071,#3056,#2650,.T.);
#3674=EDGE_CURVE('',#3072,#3071,#338,.T.);
#3675=EDGE_CURVE('',#3057,#3072,#2651,.T.);
#3676=EDGE_CURVE('',#3072,#3073,#2652,.T.);
#3677=EDGE_CURVE('',#3073,#3058,#2653,.T.);
#3678=EDGE_CURVE('',#3074,#3073,#339,.T.);
#3679=EDGE_CURVE('',#3059,#3074,#2654,.T.);
#3680=EDGE_CURVE('',#3074,#3075,#2655,.T.);
#3681=EDGE_CURVE('',#3075,#3060,#2656,.T.);
#3682=EDGE_CURVE('',#3076,#3075,#340,.T.);
#3683=EDGE_CURVE('',#3061,#3076,#2657,.T.);
#3684=EDGE_CURVE('',#3077,#3077,#2658,.T.);
#3685=EDGE_CURVE('',#3077,#3070,#1934,.T.);
#3686=EDGE_CURVE('',#3078,#3045,#2659,.T.);
#3687=EDGE_CURVE('',#3078,#3079,#341,.T.);
#3688=EDGE_CURVE('',#3076,#3079,#2660,.T.);
#3689=EDGE_CURVE('',#3063,#3078,#2661,.T.);
#3690=EDGE_CURVE('',#3079,#3062,#2662,.T.);
#3691=EDGE_CURVE('',#3080,#3080,#2663,.T.);
#3692=EDGE_CURVE('',#3081,#3081,#2664,.T.);
#3693=EDGE_CURVE('',#3082,#3082,#2665,.T.);
#3694=EDGE_CURVE('',#3082,#3080,#1935,.T.);
#3695=EDGE_CURVE('',#3083,#3083,#2666,.T.);
#3696=EDGE_CURVE('',#3083,#3081,#1936,.T.);
#3697=EDGE_CURVE('',#3084,#3084,#2667,.T.);
#3698=EDGE_CURVE('',#3085,#3085,#2668,.T.);
#3699=EDGE_CURVE('',#3086,#3086,#2669,.T.);
#3700=EDGE_CURVE('',#3086,#3084,#1937,.T.);
#3701=EDGE_CURVE('',#3087,#3087,#2670,.T.);
#3702=EDGE_CURVE('',#3087,#3085,#1938,.T.);
#3703=EDGE_CURVE('',#3088,#3088,#2671,.T.);
#3704=EDGE_CURVE('',#3088,#3089,#1939,.T.);
#3705=EDGE_CURVE('',#3089,#3089,#2672,.T.);
#3706=EDGE_CURVE('',#3090,#3090,#2673,.T.);
#3707=EDGE_CURVE('',#3090,#3091,#1940,.T.);
#3708=EDGE_CURVE('',#3091,#3091,#2674,.T.);
#3709=EDGE_CURVE('',#3092,#3093,#1941,.T.);
#3710=EDGE_CURVE('',#3092,#3094,#2675,.T.);
#3711=EDGE_CURVE('',#3095,#3094,#1942,.T.);
#3712=EDGE_CURVE('',#3093,#3095,#2676,.T.);
#3713=EDGE_CURVE('',#3096,#3093,#1943,.T.);
#3714=EDGE_CURVE('',#3097,#3096,#1944,.T.);
#3715=EDGE_CURVE('',#3092,#3097,#1945,.T.);
#3716=EDGE_CURVE('',#3095,#3098,#1946,.T.);
#3717=EDGE_CURVE('',#3098,#3096,#2677,.T.);
#3718=EDGE_CURVE('',#3099,#3099,#2678,.T.);
#3719=EDGE_CURVE('',#3100,#3094,#1947,.T.);
#3720=EDGE_CURVE('',#3098,#3100,#1948,.T.);
#3721=EDGE_CURVE('',#3100,#3097,#2679,.T.);
#3722=EDGE_CURVE('',#3101,#3101,#2680,.T.);
#3723=EDGE_CURVE('',#3102,#3102,#2681,.T.);
#3724=EDGE_CURVE('',#3103,#3103,#2682,.T.);
#3725=EDGE_CURVE('',#3101,#3102,#1949,.T.);
#3726=EDGE_CURVE('',#3103,#3104,#1950,.T.);
#3727=EDGE_CURVE('',#3104,#3104,#2683,.T.);
#3728=EDGE_CURVE('',#3105,#3105,#2684,.T.);
#3729=EDGE_CURVE('',#3105,#3099,#1951,.T.);
#3730=EDGE_CURVE('',#3106,#3106,#2685,.T.);
#3731=EDGE_CURVE('',#3106,#3107,#1952,.T.);
#3732=EDGE_CURVE('',#3107,#3107,#2686,.T.);
#3733=EDGE_CURVE('',#3108,#3108,#2687,.T.);
#3734=EDGE_CURVE('',#3108,#3109,#1953,.T.);
#3735=EDGE_CURVE('',#3109,#3109,#2688,.T.);
#3736=EDGE_CURVE('',#3110,#3110,#2689,.T.);
#3737=EDGE_CURVE('',#3110,#3111,#1954,.T.);
#3738=EDGE_CURVE('',#3111,#3111,#2690,.T.);
#3739=EDGE_CURVE('',#3112,#3112,#2691,.T.);
#3740=EDGE_CURVE('',#3112,#3113,#1955,.T.);
#3741=EDGE_CURVE('',#3113,#3113,#2692,.T.);
#3742=EDGE_CURVE('',#3114,#3115,#1956,.T.);
#3743=EDGE_CURVE('',#3114,#3115,#2693,.T.);
#3744=EDGE_CURVE('',#3116,#3114,#342,.T.);
#3745=EDGE_CURVE('',#3117,#3116,#2694,.T.);
#3746=EDGE_CURVE('',#3118,#3117,#343,.T.);
#3747=EDGE_CURVE('',#3118,#3119,#1957,.T.);
#3748=EDGE_CURVE('',#3120,#3119,#344,.T.);
#3749=EDGE_CURVE('',#3119,#3120,#345,.T.);
#3750=EDGE_CURVE('',#3115,#3118,#346,.T.);
#3751=EDGE_CURVE('',#3117,#3116,#1958,.T.);
#3752=EDGE_CURVE('',#3121,#3121,#2695,.T.);
#3753=EDGE_CURVE('',#3121,#3122,#1959,.T.);
#3754=EDGE_CURVE('',#3122,#3122,#2696,.T.);
#3755=EDGE_CURVE('',#3123,#3123,#2697,.T.);
#3756=EDGE_CURVE('',#3123,#3124,#1960,.T.);
#3757=EDGE_CURVE('',#3124,#3124,#2698,.T.);
#3758=EDGE_CURVE('',#3125,#3126,#1961,.T.);
#3759=EDGE_CURVE('',#3125,#3126,#2699,.T.);
#3760=EDGE_CURVE('',#3127,#3125,#347,.T.);
#3761=EDGE_CURVE('',#3128,#3127,#2700,.T.);
#3762=EDGE_CURVE('',#3129,#3128,#348,.T.);
#3763=EDGE_CURVE('',#3129,#3130,#1962,.T.);
#3764=EDGE_CURVE('',#3131,#3130,#349,.T.);
#3765=EDGE_CURVE('',#3130,#3131,#350,.T.);
#3766=EDGE_CURVE('',#3126,#3129,#351,.T.);
#3767=EDGE_CURVE('',#3128,#3127,#1963,.T.);
#3768=EDGE_CURVE('',#3132,#3132,#2701,.T.);
#3769=EDGE_CURVE('',#3132,#3133,#1964,.T.);
#3770=EDGE_CURVE('',#3133,#3133,#2702,.T.);
#3771=EDGE_CURVE('',#3134,#3134,#2703,.T.);
#3772=EDGE_CURVE('',#3134,#3135,#1965,.T.);
#3773=EDGE_CURVE('',#3135,#3135,#2704,.T.);
#3774=EDGE_CURVE('',#3136,#3136,#2705,.T.);
#3775=EDGE_CURVE('',#3136,#3137,#1966,.T.);
#3776=EDGE_CURVE('',#3137,#3137,#2706,.T.);
#3777=EDGE_CURVE('',#3138,#3138,#2707,.T.);
#3778=EDGE_CURVE('',#3138,#3139,#1967,.T.);
#3779=EDGE_CURVE('',#3139,#3139,#2708,.T.);
#3780=EDGE_CURVE('',#3140,#3140,#2709,.T.);
#3781=EDGE_CURVE('',#3140,#3141,#1968,.T.);
#3782=EDGE_CURVE('',#3141,#3141,#2710,.T.);
#3783=EDGE_CURVE('',#3142,#3142,#2711,.T.);
#3784=EDGE_CURVE('',#3142,#3143,#1969,.T.);
#3785=EDGE_CURVE('',#3143,#3143,#2712,.T.);
#3786=EDGE_CURVE('',#3144,#3144,#2713,.T.);
#3787=EDGE_CURVE('',#3145,#3145,#2714,.T.);
#3788=EDGE_CURVE('',#3146,#3146,#2715,.T.);
#3789=EDGE_CURVE('',#3147,#3147,#2716,.T.);
#3790=EDGE_CURVE('',#3144,#3146,#1970,.T.);
#3791=EDGE_CURVE('',#3147,#3148,#1971,.T.);
#3792=EDGE_CURVE('',#3148,#3148,#2717,.T.);
#3793=EDGE_CURVE('',#3149,#3149,#2718,.T.);
#3794=EDGE_CURVE('',#3149,#3145,#1972,.T.);
#3795=EDGE_CURVE('',#3150,#3150,#2719,.T.);
#3796=EDGE_CURVE('',#3150,#3151,#1973,.T.);
#3797=EDGE_CURVE('',#3151,#3151,#2720,.T.);
#3798=EDGE_CURVE('',#3152,#3152,#2721,.T.);
#3799=EDGE_CURVE('',#3152,#3153,#1974,.T.);
#3800=EDGE_CURVE('',#3153,#3153,#2722,.T.);
#3801=EDGE_CURVE('',#3154,#3154,#2723,.T.);
#3802=EDGE_CURVE('',#3154,#3155,#1975,.T.);
#3803=EDGE_CURVE('',#3155,#3155,#2724,.T.);
#3804=EDGE_CURVE('',#3156,#3156,#2725,.T.);
#3805=EDGE_CURVE('',#3156,#3157,#1976,.T.);
#3806=EDGE_CURVE('',#3157,#3157,#2726,.T.);
#3807=EDGE_CURVE('',#3158,#3158,#2727,.T.);
#3808=EDGE_CURVE('',#3158,#3159,#1977,.T.);
#3809=EDGE_CURVE('',#3159,#3159,#2728,.T.);
#3810=EDGE_CURVE('',#3160,#3160,#2729,.T.);
#3811=EDGE_CURVE('',#3160,#3161,#1978,.T.);
#3812=EDGE_CURVE('',#3161,#3161,#2730,.T.);
#3813=EDGE_CURVE('',#3162,#3162,#2731,.T.);
#3814=EDGE_CURVE('',#3162,#3163,#1979,.T.);
#3815=EDGE_CURVE('',#3163,#3163,#2732,.T.);
#3816=EDGE_CURVE('',#3164,#3164,#2733,.T.);
#3817=EDGE_CURVE('',#3164,#3165,#1980,.T.);
#3818=EDGE_CURVE('',#3165,#3165,#2734,.T.);
#3819=EDGE_CURVE('',#3166,#3167,#1981,.T.);
#3820=EDGE_CURVE('',#3166,#3168,#1982,.T.);
#3821=EDGE_CURVE('',#3168,#3169,#1983,.T.);
#3822=EDGE_CURVE('',#3167,#3169,#1984,.T.);
#3823=EDGE_CURVE('',#3170,#3166,#1985,.T.);
#3824=EDGE_CURVE('',#3170,#3171,#1986,.T.);
#3825=EDGE_CURVE('',#3171,#3168,#1987,.T.);
#3826=EDGE_CURVE('',#3172,#3170,#1988,.T.);
#3827=EDGE_CURVE('',#3172,#3173,#1989,.T.);
#3828=EDGE_CURVE('',#3173,#3171,#1990,.T.);
#3829=EDGE_CURVE('',#3174,#3172,#1991,.T.);
#3830=EDGE_CURVE('',#3174,#3175,#1992,.T.);
#3831=EDGE_CURVE('',#3175,#3173,#1993,.T.);
#3832=EDGE_CURVE('',#3176,#3174,#1994,.T.);
#3833=EDGE_CURVE('',#3176,#3177,#1995,.T.);
#3834=EDGE_CURVE('',#3177,#3175,#1996,.T.);
#3835=EDGE_CURVE('',#3167,#3176,#1997,.T.);
#3836=EDGE_CURVE('',#3169,#3177,#1998,.T.);
#3837=EDGE_CURVE('',#3178,#3178,#2735,.T.);
#3838=EDGE_CURVE('',#3179,#3179,#2736,.T.);
#3839=EDGE_CURVE('',#3179,#3178,#1999,.T.);
#3840=EDGE_CURVE('',#3180,#3180,#2737,.F.);
#3841=EDGE_CURVE('',#3180,#3179,#2000,.T.);
#3842=EDGE_CURVE('',#3181,#3181,#2738,.T.);
#3843=EDGE_CURVE('',#3181,#3180,#2001,.T.);
#3844=EDGE_CURVE('',#3182,#3182,#2739,.T.);
#3845=EDGE_CURVE('',#3182,#3183,#2002,.T.);
#3846=EDGE_CURVE('',#3183,#3183,#2740,.T.);
#3847=EDGE_CURVE('',#3184,#3184,#2741,.T.);
#3848=EDGE_CURVE('',#3184,#3185,#2003,.T.);
#3849=EDGE_CURVE('',#3185,#3185,#2742,.T.);
#3850=EDGE_CURVE('',#3186,#3186,#2743,.T.);
#3851=EDGE_CURVE('',#3186,#3187,#2004,.T.);
#3852=EDGE_CURVE('',#3187,#3187,#2744,.T.);
#3853=EDGE_CURVE('',#3188,#3188,#2745,.T.);
#3854=EDGE_CURVE('',#3188,#3189,#2005,.T.);
#3855=EDGE_CURVE('',#3189,#3189,#2746,.T.);
#3856=EDGE_CURVE('',#3190,#3191,#2006,.T.);
#3857=EDGE_CURVE('',#3192,#3190,#2007,.T.);
#3858=EDGE_CURVE('',#3193,#3192,#2008,.T.);
#3859=EDGE_CURVE('',#3191,#3193,#2009,.T.);
#3860=EDGE_CURVE('',#3194,#3194,#2747,.T.);
#3861=EDGE_CURVE('',#3190,#3195,#2010,.T.);
#3862=EDGE_CURVE('',#3196,#3195,#2011,.T.);
#3863=EDGE_CURVE('',#3192,#3196,#2012,.T.);
#3864=EDGE_CURVE('',#3197,#3196,#2013,.T.);
#3865=EDGE_CURVE('',#3193,#3197,#2014,.T.);
#3866=EDGE_CURVE('',#3198,#3197,#2015,.T.);
#3867=EDGE_CURVE('',#3191,#3198,#2016,.T.);
#3868=EDGE_CURVE('',#3195,#3198,#2017,.T.);
#3869=EDGE_CURVE('',#3194,#3199,#2018,.T.);
#3870=EDGE_CURVE('',#3199,#3199,#2748,.T.);
#3871=EDGE_CURVE('',#3200,#3200,#2749,.T.);
#3872=EDGE_CURVE('',#3200,#3201,#2019,.T.);
#3873=EDGE_CURVE('',#3201,#3201,#2750,.T.);
#3874=EDGE_CURVE('',#3202,#3203,#2020,.T.);
#3875=EDGE_CURVE('',#3202,#3204,#2751,.T.);
#3876=EDGE_CURVE('',#3205,#3204,#2021,.T.);
#3877=EDGE_CURVE('',#3203,#3205,#2752,.T.);
#3878=EDGE_CURVE('',#3206,#3203,#2022,.T.);
#3879=EDGE_CURVE('',#3207,#3206,#2023,.T.);
#3880=EDGE_CURVE('',#3202,#3207,#2024,.T.);
#3881=EDGE_CURVE('',#3205,#3208,#2025,.T.);
#3882=EDGE_CURVE('',#3208,#3206,#2753,.T.);
#3883=EDGE_CURVE('',#3209,#3204,#2026,.T.);
#3884=EDGE_CURVE('',#3208,#3209,#2027,.T.);
#3885=EDGE_CURVE('',#3209,#3207,#2754,.T.);
#3886=EDGE_CURVE('',#3210,#3210,#2755,.T.);
#3887=EDGE_CURVE('',#3211,#3211,#2756,.T.);
#3888=EDGE_CURVE('',#3212,#3212,#2757,.T.);
#3889=EDGE_CURVE('',#3210,#3211,#2028,.T.);
#3890=EDGE_CURVE('',#3212,#3213,#2029,.T.);
#3891=EDGE_CURVE('',#3213,#3213,#2758,.T.);
#3892=EDGE_CURVE('',#3214,#3214,#2759,.T.);
#3893=EDGE_CURVE('',#3214,#3215,#2030,.T.);
#3894=EDGE_CURVE('',#3215,#3215,#2760,.T.);
#3895=EDGE_CURVE('',#3216,#3216,#2761,.T.);
#3896=EDGE_CURVE('',#3216,#3217,#2031,.T.);
#3897=EDGE_CURVE('',#3217,#3217,#2762,.T.);
#3898=EDGE_CURVE('',#3218,#3219,#2032,.T.);
#3899=EDGE_CURVE('',#3218,#3219,#2763,.T.);
#3900=EDGE_CURVE('',#3220,#3218,#352,.T.);
#3901=EDGE_CURVE('',#3221,#3220,#2764,.T.);
#3902=EDGE_CURVE('',#3222,#3221,#353,.T.);
#3903=EDGE_CURVE('',#3222,#3223,#2033,.T.);
#3904=EDGE_CURVE('',#3224,#3223,#354,.T.);
#3905=EDGE_CURVE('',#3223,#3224,#355,.T.);
#3906=EDGE_CURVE('',#3219,#3222,#356,.T.);
#3907=EDGE_CURVE('',#3221,#3220,#2034,.T.);
#3908=EDGE_CURVE('',#3225,#3225,#2765,.T.);
#3909=EDGE_CURVE('',#3225,#3226,#2035,.T.);
#3910=EDGE_CURVE('',#3226,#3226,#2766,.T.);
#3911=EDGE_CURVE('',#3227,#3227,#2767,.T.);
#3912=EDGE_CURVE('',#3227,#3228,#2036,.T.);
#3913=EDGE_CURVE('',#3228,#3228,#2768,.T.);
#3914=EDGE_CURVE('',#3229,#3229,#2769,.T.);
#3915=EDGE_CURVE('',#3229,#3230,#2037,.T.);
#3916=EDGE_CURVE('',#3230,#3230,#2770,.T.);
#3917=EDGE_CURVE('',#3231,#3231,#2771,.T.);
#3918=EDGE_CURVE('',#3231,#3232,#2038,.T.);
#3919=EDGE_CURVE('',#3232,#3232,#2772,.T.);
#3920=EDGE_CURVE('',#3233,#3233,#2773,.T.);
#3921=EDGE_CURVE('',#3234,#3234,#2774,.T.);
#3922=EDGE_CURVE('',#3235,#3235,#2775,.T.);
#3923=EDGE_CURVE('',#3236,#3236,#2776,.T.);
#3924=EDGE_CURVE('',#3233,#3235,#2039,.T.);
#3925=EDGE_CURVE('',#3236,#3237,#2040,.T.);
#3926=EDGE_CURVE('',#3237,#3237,#2777,.T.);
#3927=EDGE_CURVE('',#3238,#3238,#2778,.T.);
#3928=EDGE_CURVE('',#3238,#3234,#2041,.T.);
#3929=EDGE_CURVE('',#3239,#3239,#2779,.T.);
#3930=EDGE_CURVE('',#3239,#3240,#2042,.T.);
#3931=EDGE_CURVE('',#3240,#3240,#2780,.T.);
#3932=EDGE_CURVE('',#3241,#3241,#2781,.T.);
#3933=EDGE_CURVE('',#3241,#3242,#2043,.T.);
#3934=EDGE_CURVE('',#3242,#3242,#2782,.T.);
#3935=EDGE_CURVE('',#3243,#3243,#2783,.T.);
#3936=EDGE_CURVE('',#3243,#3244,#2044,.T.);
#3937=EDGE_CURVE('',#3244,#3244,#2784,.T.);
#3938=EDGE_CURVE('',#3245,#3245,#2785,.T.);
#3939=EDGE_CURVE('',#3245,#3246,#2045,.T.);
#3940=EDGE_CURVE('',#3246,#3246,#2786,.T.);
#3941=EDGE_CURVE('',#3247,#3247,#2787,.T.);
#3942=EDGE_CURVE('',#3247,#3248,#2046,.T.);
#3943=EDGE_CURVE('',#3248,#3248,#2788,.T.);
#3944=EDGE_CURVE('',#3249,#3249,#2789,.T.);
#3945=EDGE_CURVE('',#3249,#3250,#2047,.T.);
#3946=EDGE_CURVE('',#3250,#3250,#2790,.T.);
#3947=EDGE_CURVE('',#3251,#3251,#2791,.T.);
#3948=EDGE_CURVE('',#3251,#3252,#2048,.T.);
#3949=EDGE_CURVE('',#3252,#3252,#2792,.T.);
#3950=EDGE_CURVE('',#3253,#3253,#2793,.T.);
#3951=EDGE_CURVE('',#3253,#3254,#2049,.T.);
#3952=EDGE_CURVE('',#3254,#3254,#2794,.T.);
#3953=EDGE_CURVE('',#3255,#3255,#2795,.T.);
#3954=EDGE_CURVE('',#3256,#3257,#2050,.T.);
#3955=EDGE_CURVE('',#3256,#3258,#2051,.T.);
#3956=EDGE_CURVE('',#3258,#3259,#2052,.T.);
#3957=EDGE_CURVE('',#3257,#3259,#2053,.T.);
#3958=EDGE_CURVE('',#3260,#3256,#2054,.T.);
#3959=EDGE_CURVE('',#3260,#3261,#2055,.T.);
#3960=EDGE_CURVE('',#3261,#3258,#2056,.T.);
#3961=EDGE_CURVE('',#3262,#3260,#2057,.T.);
#3962=EDGE_CURVE('',#3262,#3263,#2058,.T.);
#3963=EDGE_CURVE('',#3263,#3261,#2059,.T.);
#3964=EDGE_CURVE('',#3264,#3262,#2060,.T.);
#3965=EDGE_CURVE('',#3264,#3265,#2061,.T.);
#3966=EDGE_CURVE('',#3265,#3263,#2062,.T.);
#3967=EDGE_CURVE('',#3266,#3264,#2063,.T.);
#3968=EDGE_CURVE('',#3266,#3267,#2064,.T.);
#3969=EDGE_CURVE('',#3267,#3265,#2065,.T.);
#3970=EDGE_CURVE('',#3257,#3266,#2066,.T.);
#3971=EDGE_CURVE('',#3259,#3267,#2067,.T.);
#3972=EDGE_CURVE('',#3268,#3268,#2796,.T.);
#3973=EDGE_CURVE('',#3269,#3269,#2797,.T.);
#3974=EDGE_CURVE('',#3269,#3268,#2068,.T.);
#3975=EDGE_CURVE('',#3255,#3269,#2069,.T.);
#3976=EDGE_CURVE('',#3270,#3270,#2798,.T.);
#3977=EDGE_CURVE('',#3271,#3271,#2799,.T.);
#3978=EDGE_CURVE('',#3271,#3270,#2070,.T.);
#3979=EDGE_CURVE('',#3272,#3272,#2800,.T.);
#3980=EDGE_CURVE('',#3272,#3271,#2071,.T.);
#3981=EDGE_CURVE('',#3273,#3273,#2801,.T.);
#3982=EDGE_CURVE('',#3273,#3272,#2072,.T.);
#3983=EDGE_CURVE('',#3274,#3274,#2802,.T.);
#3984=EDGE_CURVE('',#3275,#3275,#2803,.F.);
#3985=EDGE_CURVE('',#3275,#3274,#2073,.T.);
#3986=EDGE_CURVE('',#3276,#3276,#2804,.F.);
#3987=EDGE_CURVE('',#3276,#3275,#2074,.T.);
#3988=EDGE_CURVE('',#3277,#3277,#2805,.T.);
#3989=EDGE_CURVE('',#3277,#3276,#2075,.T.);
#3990=EDGE_CURVE('',#3278,#3279,#2076,.T.);
#3991=EDGE_CURVE('',#3279,#3280,#2077,.T.);
#3992=EDGE_CURVE('',#3280,#3281,#2078,.T.);
#3993=EDGE_CURVE('',#3278,#3281,#2079,.T.);
#3994=EDGE_CURVE('',#3279,#3282,#2080,.T.);
#3995=EDGE_CURVE('',#3282,#3283,#2081,.T.);
#3996=EDGE_CURVE('',#3283,#3280,#2082,.T.);
#3997=EDGE_CURVE('',#3282,#3284,#2083,.T.);
#3998=EDGE_CURVE('',#3284,#3285,#2084,.T.);
#3999=EDGE_CURVE('',#3285,#3283,#2085,.T.);
#4000=EDGE_CURVE('',#3284,#3286,#2086,.T.);
#4001=EDGE_CURVE('',#3286,#3287,#2087,.T.);
#4002=EDGE_CURVE('',#3287,#3285,#2088,.T.);
#4003=EDGE_CURVE('',#3286,#3288,#2089,.T.);
#4004=EDGE_CURVE('',#3288,#3289,#2090,.T.);
#4005=EDGE_CURVE('',#3289,#3287,#2091,.T.);
#4006=EDGE_CURVE('',#3288,#3278,#2092,.T.);
#4007=EDGE_CURVE('',#3281,#3289,#2093,.T.);
#4008=EDGE_CURVE('',#3290,#3291,#2094,.T.);
#4009=EDGE_CURVE('',#3291,#3292,#2095,.T.);
#4010=EDGE_CURVE('',#3292,#3293,#2096,.T.);
#4011=EDGE_CURVE('',#3290,#3293,#2097,.T.);
#4012=EDGE_CURVE('',#3291,#3294,#2098,.T.);
#4013=EDGE_CURVE('',#3294,#3295,#2099,.T.);
#4014=EDGE_CURVE('',#3295,#3292,#2100,.T.);
#4015=EDGE_CURVE('',#3294,#3296,#2101,.T.);
#4016=EDGE_CURVE('',#3296,#3297,#2102,.T.);
#4017=EDGE_CURVE('',#3297,#3295,#2103,.T.);
#4018=EDGE_CURVE('',#3296,#3298,#2104,.T.);
#4019=EDGE_CURVE('',#3298,#3299,#2105,.T.);
#4020=EDGE_CURVE('',#3299,#3297,#2106,.T.);
#4021=EDGE_CURVE('',#3298,#3300,#2107,.T.);
#4022=EDGE_CURVE('',#3300,#3301,#2108,.T.);
#4023=EDGE_CURVE('',#3301,#3299,#2109,.T.);
#4024=EDGE_CURVE('',#3300,#3290,#2110,.T.);
#4025=EDGE_CURVE('',#3293,#3301,#2111,.T.);
#4026=EDGE_CURVE('',#3302,#3302,#2806,.T.);
#4027=EDGE_CURVE('',#3303,#3303,#2807,.T.);
#4028=EDGE_CURVE('',#3304,#3304,#2808,.T.);
#4029=EDGE_CURVE('',#3304,#3303,#2112,.T.);
#4030=EDGE_CURVE('',#3305,#3305,#2809,.T.);
#4031=EDGE_CURVE('',#3305,#3304,#2113,.T.);
#4032=EDGE_CURVE('',#3306,#3306,#2810,.T.);
#4033=EDGE_CURVE('',#3306,#3305,#2114,.T.);
#4034=EDGE_CURVE('',#3307,#3307,#2811,.T.);
#4035=EDGE_CURVE('',#3308,#3308,#2812,.F.);
#4036=EDGE_CURVE('',#3308,#3307,#2115,.T.);
#4037=EDGE_CURVE('',#3302,#3308,#2116,.T.);
#4038=EDGE_CURVE('',#3309,#3309,#2813,.T.);
#4039=EDGE_CURVE('',#3309,#3310,#2117,.T.);
#4040=EDGE_CURVE('',#3310,#3310,#2814,.T.);
#4041=EDGE_CURVE('',#3311,#3311,#2815,.T.);
#4042=EDGE_CURVE('',#3311,#3312,#2118,.T.);
#4043=EDGE_CURVE('',#3312,#3312,#2816,.T.);
#4044=EDGE_CURVE('',#3313,#3314,#2119,.T.);
#4045=EDGE_CURVE('',#3315,#3313,#2817,.T.);
#4046=EDGE_CURVE('',#3316,#3315,#2120,.T.);
#4047=EDGE_CURVE('',#3316,#3314,#2818,.T.);
#4048=EDGE_CURVE('',#3317,#3314,#2121,.T.);
#4049=EDGE_CURVE('',#3318,#3317,#2122,.T.);
#4050=EDGE_CURVE('',#3313,#3318,#2123,.T.);
#4051=EDGE_CURVE('',#3316,#3319,#2124,.T.);
#4052=EDGE_CURVE('',#3317,#3319,#2819,.T.);
#4053=EDGE_CURVE('',#3320,#3315,#2125,.T.);
#4054=EDGE_CURVE('',#3319,#3320,#2126,.T.);
#4055=EDGE_CURVE('',#3318,#3320,#2820,.T.);
#4056=EDGE_CURVE('',#3321,#3321,#2821,.T.);
#4057=EDGE_CURVE('',#3321,#3322,#2127,.T.);
#4058=EDGE_CURVE('',#3322,#3322,#2822,.T.);
#4059=EDGE_CURVE('',#3323,#3323,#2823,.T.);
#4060=EDGE_CURVE('',#3323,#3324,#2128,.T.);
#4061=EDGE_CURVE('',#3324,#3324,#2824,.T.);
#4062=EDGE_CURVE('',#3325,#3325,#2825,.T.);
#4063=EDGE_CURVE('',#3325,#3326,#2129,.T.);
#4064=EDGE_CURVE('',#3326,#3326,#2826,.T.);
#4065=EDGE_CURVE('',#3327,#3327,#2827,.T.);
#4066=EDGE_CURVE('',#3327,#3328,#2130,.T.);
#4067=EDGE_CURVE('',#3328,#3328,#2828,.T.);
#4068=ORIENTED_EDGE('',*,*,#3329,.F.);
#4069=ORIENTED_EDGE('',*,*,#3330,.T.);
#4070=ORIENTED_EDGE('',*,*,#3331,.F.);
#4071=ORIENTED_EDGE('',*,*,#3330,.F.);
#4072=ORIENTED_EDGE('',*,*,#3332,.F.);
#4073=ORIENTED_EDGE('',*,*,#3333,.T.);
#4074=ORIENTED_EDGE('',*,*,#3334,.F.);
#4075=ORIENTED_EDGE('',*,*,#3333,.F.);
#4076=ORIENTED_EDGE('',*,*,#3335,.F.);
#4077=ORIENTED_EDGE('',*,*,#3336,.T.);
#4078=ORIENTED_EDGE('',*,*,#3337,.F.);
#4079=ORIENTED_EDGE('',*,*,#3336,.F.);
#4080=ORIENTED_EDGE('',*,*,#3338,.F.);
#4081=ORIENTED_EDGE('',*,*,#3339,.T.);
#4082=ORIENTED_EDGE('',*,*,#3340,.F.);
#4083=ORIENTED_EDGE('',*,*,#3339,.F.);
#4084=ORIENTED_EDGE('',*,*,#3341,.F.);
#4085=ORIENTED_EDGE('',*,*,#3342,.T.);
#4086=ORIENTED_EDGE('',*,*,#3343,.F.);
#4087=ORIENTED_EDGE('',*,*,#3342,.F.);
#4088=ORIENTED_EDGE('',*,*,#3344,.F.);
#4089=ORIENTED_EDGE('',*,*,#3345,.T.);
#4090=ORIENTED_EDGE('',*,*,#3346,.F.);
#4091=ORIENTED_EDGE('',*,*,#3345,.F.);
#4092=ORIENTED_EDGE('',*,*,#3347,.F.);
#4093=ORIENTED_EDGE('',*,*,#3348,.T.);
#4094=ORIENTED_EDGE('',*,*,#3349,.F.);
#4095=ORIENTED_EDGE('',*,*,#3348,.F.);
#4096=ORIENTED_EDGE('',*,*,#3350,.F.);
#4097=ORIENTED_EDGE('',*,*,#3351,.T.);
#4098=ORIENTED_EDGE('',*,*,#3352,.F.);
#4099=ORIENTED_EDGE('',*,*,#3351,.F.);
#4100=ORIENTED_EDGE('',*,*,#3353,.T.);
#4101=ORIENTED_EDGE('',*,*,#3354,.T.);
#4102=ORIENTED_EDGE('',*,*,#3355,.F.);
#4103=ORIENTED_EDGE('',*,*,#3356,.F.);
#4104=ORIENTED_EDGE('',*,*,#3357,.T.);
#4105=ORIENTED_EDGE('',*,*,#3356,.T.);
#4106=ORIENTED_EDGE('',*,*,#3358,.F.);
#4107=ORIENTED_EDGE('',*,*,#3359,.F.);
#4108=ORIENTED_EDGE('',*,*,#3360,.T.);
#4109=ORIENTED_EDGE('',*,*,#3359,.T.);
#4110=ORIENTED_EDGE('',*,*,#3361,.F.);
#4111=ORIENTED_EDGE('',*,*,#3362,.F.);
#4112=ORIENTED_EDGE('',*,*,#3363,.T.);
#4113=ORIENTED_EDGE('',*,*,#3362,.T.);
#4114=ORIENTED_EDGE('',*,*,#3364,.F.);
#4115=ORIENTED_EDGE('',*,*,#3354,.F.);
#4116=ORIENTED_EDGE('',*,*,#3364,.T.);
#4117=ORIENTED_EDGE('',*,*,#3361,.T.);
#4118=ORIENTED_EDGE('',*,*,#3358,.T.);
#4119=ORIENTED_EDGE('',*,*,#3355,.T.);
#4120=ORIENTED_EDGE('',*,*,#3352,.T.);
#4121=ORIENTED_EDGE('',*,*,#3349,.T.);
#4122=ORIENTED_EDGE('',*,*,#3346,.T.);
#4123=ORIENTED_EDGE('',*,*,#3343,.T.);
#4124=ORIENTED_EDGE('',*,*,#3340,.T.);
#4125=ORIENTED_EDGE('',*,*,#3337,.T.);
#4126=ORIENTED_EDGE('',*,*,#3334,.T.);
#4127=ORIENTED_EDGE('',*,*,#3331,.T.);
#4128=ORIENTED_EDGE('',*,*,#3363,.F.);
#4129=ORIENTED_EDGE('',*,*,#3353,.F.);
#4130=ORIENTED_EDGE('',*,*,#3357,.F.);
#4131=ORIENTED_EDGE('',*,*,#3360,.F.);
#4132=ORIENTED_EDGE('',*,*,#3350,.T.);
#4133=ORIENTED_EDGE('',*,*,#3347,.T.);
#4134=ORIENTED_EDGE('',*,*,#3344,.T.);
#4135=ORIENTED_EDGE('',*,*,#3341,.T.);
#4136=ORIENTED_EDGE('',*,*,#3338,.T.);
#4137=ORIENTED_EDGE('',*,*,#3335,.T.);
#4138=ORIENTED_EDGE('',*,*,#3332,.T.);
#4139=ORIENTED_EDGE('',*,*,#3329,.T.);
#4140=ORIENTED_EDGE('',*,*,#3365,.T.);
#4141=ORIENTED_EDGE('',*,*,#3366,.T.);
#4142=ORIENTED_EDGE('',*,*,#3367,.F.);
#4143=ORIENTED_EDGE('',*,*,#3368,.F.);
#4144=ORIENTED_EDGE('',*,*,#3369,.T.);
#4145=ORIENTED_EDGE('',*,*,#3368,.T.);
#4146=ORIENTED_EDGE('',*,*,#3370,.F.);
#4147=ORIENTED_EDGE('',*,*,#3371,.F.);
#4148=ORIENTED_EDGE('',*,*,#3372,.T.);
#4149=ORIENTED_EDGE('',*,*,#3371,.T.);
#4150=ORIENTED_EDGE('',*,*,#3373,.F.);
#4151=ORIENTED_EDGE('',*,*,#3374,.F.);
#4152=ORIENTED_EDGE('',*,*,#3375,.T.);
#4153=ORIENTED_EDGE('',*,*,#3374,.T.);
#4154=ORIENTED_EDGE('',*,*,#3376,.F.);
#4155=ORIENTED_EDGE('',*,*,#3366,.F.);
#4156=ORIENTED_EDGE('',*,*,#3376,.T.);
#4157=ORIENTED_EDGE('',*,*,#3373,.T.);
#4158=ORIENTED_EDGE('',*,*,#3370,.T.);
#4159=ORIENTED_EDGE('',*,*,#3367,.T.);
#4160=ORIENTED_EDGE('',*,*,#3375,.F.);
#4161=ORIENTED_EDGE('',*,*,#3365,.F.);
#4162=ORIENTED_EDGE('',*,*,#3369,.F.);
#4163=ORIENTED_EDGE('',*,*,#3372,.F.);
#4164=ORIENTED_EDGE('',*,*,#3377,.T.);
#4165=ORIENTED_EDGE('',*,*,#3378,.T.);
#4166=ORIENTED_EDGE('',*,*,#3379,.F.);
#4167=ORIENTED_EDGE('',*,*,#3380,.F.);
#4168=ORIENTED_EDGE('',*,*,#3381,.T.);
#4169=ORIENTED_EDGE('',*,*,#3380,.T.);
#4170=ORIENTED_EDGE('',*,*,#3382,.F.);
#4171=ORIENTED_EDGE('',*,*,#3383,.F.);
#4172=ORIENTED_EDGE('',*,*,#3384,.T.);
#4173=ORIENTED_EDGE('',*,*,#3383,.T.);
#4174=ORIENTED_EDGE('',*,*,#3385,.F.);
#4175=ORIENTED_EDGE('',*,*,#3386,.F.);
#4176=ORIENTED_EDGE('',*,*,#3387,.T.);
#4177=ORIENTED_EDGE('',*,*,#3386,.T.);
#4178=ORIENTED_EDGE('',*,*,#3388,.F.);
#4179=ORIENTED_EDGE('',*,*,#3378,.F.);
#4180=ORIENTED_EDGE('',*,*,#3388,.T.);
#4181=ORIENTED_EDGE('',*,*,#3385,.T.);
#4182=ORIENTED_EDGE('',*,*,#3382,.T.);
#4183=ORIENTED_EDGE('',*,*,#3379,.T.);
#4184=ORIENTED_EDGE('',*,*,#3387,.F.);
#4185=ORIENTED_EDGE('',*,*,#3377,.F.);
#4186=ORIENTED_EDGE('',*,*,#3381,.F.);
#4187=ORIENTED_EDGE('',*,*,#3384,.F.);
#4188=ORIENTED_EDGE('',*,*,#3389,.F.);
#4189=ORIENTED_EDGE('',*,*,#3390,.F.);
#4190=ORIENTED_EDGE('',*,*,#3391,.F.);
#4191=ORIENTED_EDGE('',*,*,#3392,.F.);
#4192=ORIENTED_EDGE('',*,*,#3393,.F.);
#4193=ORIENTED_EDGE('',*,*,#3390,.T.);
#4194=ORIENTED_EDGE('',*,*,#3394,.F.);
#4195=ORIENTED_EDGE('',*,*,#3395,.T.);
#4196=ORIENTED_EDGE('',*,*,#3396,.F.);
#4197=ORIENTED_EDGE('',*,*,#3397,.F.);
#4198=ORIENTED_EDGE('',*,*,#3398,.F.);
#4199=ORIENTED_EDGE('',*,*,#3395,.F.);
#4200=ORIENTED_EDGE('',*,*,#3399,.F.);
#4201=ORIENTED_EDGE('',*,*,#3400,.T.);
#4202=ORIENTED_EDGE('',*,*,#3401,.F.);
#4203=ORIENTED_EDGE('',*,*,#3402,.F.);
#4204=ORIENTED_EDGE('',*,*,#3403,.F.);
#4205=ORIENTED_EDGE('',*,*,#3400,.F.);
#4206=ORIENTED_EDGE('',*,*,#3404,.F.);
#4207=ORIENTED_EDGE('',*,*,#3405,.T.);
#4208=ORIENTED_EDGE('',*,*,#3406,.F.);
#4209=ORIENTED_EDGE('',*,*,#3407,.F.);
#4210=ORIENTED_EDGE('',*,*,#3408,.F.);
#4211=ORIENTED_EDGE('',*,*,#3405,.F.);
#4212=ORIENTED_EDGE('',*,*,#3409,.F.);
#4213=ORIENTED_EDGE('',*,*,#3410,.T.);
#4214=ORIENTED_EDGE('',*,*,#3411,.T.);
#4215=ORIENTED_EDGE('',*,*,#3391,.T.);
#4216=ORIENTED_EDGE('',*,*,#3389,.T.);
#4217=ORIENTED_EDGE('',*,*,#3393,.T.);
#4218=ORIENTED_EDGE('',*,*,#3412,.T.);
#4219=ORIENTED_EDGE('',*,*,#3406,.T.);
#4220=ORIENTED_EDGE('',*,*,#3408,.T.);
#4221=ORIENTED_EDGE('',*,*,#3404,.T.);
#4222=ORIENTED_EDGE('',*,*,#3413,.T.);
#4223=ORIENTED_EDGE('',*,*,#3401,.T.);
#4224=ORIENTED_EDGE('',*,*,#3403,.T.);
#4225=ORIENTED_EDGE('',*,*,#3399,.T.);
#4226=ORIENTED_EDGE('',*,*,#3414,.T.);
#4227=ORIENTED_EDGE('',*,*,#3396,.T.);
#4228=ORIENTED_EDGE('',*,*,#3398,.T.);
#4229=ORIENTED_EDGE('',*,*,#3394,.T.);
#4230=ORIENTED_EDGE('',*,*,#3415,.T.);
#4231=ORIENTED_EDGE('',*,*,#3410,.F.);
#4232=ORIENTED_EDGE('',*,*,#3416,.T.);
#4233=ORIENTED_EDGE('',*,*,#3415,.F.);
#4234=ORIENTED_EDGE('',*,*,#3397,.T.);
#4235=ORIENTED_EDGE('',*,*,#3414,.F.);
#4236=ORIENTED_EDGE('',*,*,#3402,.T.);
#4237=ORIENTED_EDGE('',*,*,#3413,.F.);
#4238=ORIENTED_EDGE('',*,*,#3407,.T.);
#4239=ORIENTED_EDGE('',*,*,#3412,.F.);
#4240=ORIENTED_EDGE('',*,*,#3392,.T.);
#4241=ORIENTED_EDGE('',*,*,#3411,.F.);
#4242=ORIENTED_EDGE('',*,*,#3417,.T.);
#4243=ORIENTED_EDGE('',*,*,#3418,.T.);
#4244=ORIENTED_EDGE('',*,*,#3419,.T.);
#4245=ORIENTED_EDGE('',*,*,#3420,.T.);
#4246=ORIENTED_EDGE('',*,*,#3421,.F.);
#4247=ORIENTED_EDGE('',*,*,#3422,.T.);
#4248=ORIENTED_EDGE('',*,*,#3423,.F.);
#4249=ORIENTED_EDGE('',*,*,#3422,.F.);
#4250=ORIENTED_EDGE('',*,*,#3421,.T.);
#4251=ORIENTED_EDGE('',*,*,#3424,.F.);
#4252=ORIENTED_EDGE('',*,*,#3425,.T.);
#4253=ORIENTED_EDGE('',*,*,#3426,.F.);
#4254=ORIENTED_EDGE('',*,*,#3425,.F.);
#4255=ORIENTED_EDGE('',*,*,#3424,.T.);
#4256=ORIENTED_EDGE('',*,*,#3427,.F.);
#4257=ORIENTED_EDGE('',*,*,#3428,.T.);
#4258=ORIENTED_EDGE('',*,*,#3429,.F.);
#4259=ORIENTED_EDGE('',*,*,#3428,.F.);
#4260=ORIENTED_EDGE('',*,*,#3427,.T.);
#4261=ORIENTED_EDGE('',*,*,#3430,.F.);
#4262=ORIENTED_EDGE('',*,*,#3431,.T.);
#4263=ORIENTED_EDGE('',*,*,#3432,.F.);
#4264=ORIENTED_EDGE('',*,*,#3431,.F.);
#4265=ORIENTED_EDGE('',*,*,#3430,.T.);
#4266=ORIENTED_EDGE('',*,*,#3433,.F.);
#4267=ORIENTED_EDGE('',*,*,#3434,.F.);
#4268=ORIENTED_EDGE('',*,*,#3435,.T.);
#4269=ORIENTED_EDGE('',*,*,#3436,.F.);
#4270=ORIENTED_EDGE('',*,*,#3437,.F.);
#4271=ORIENTED_EDGE('',*,*,#3435,.F.);
#4272=ORIENTED_EDGE('',*,*,#3438,.F.);
#4273=ORIENTED_EDGE('',*,*,#3439,.T.);
#4274=ORIENTED_EDGE('',*,*,#3417,.F.);
#4275=ORIENTED_EDGE('',*,*,#3439,.F.);
#4276=ORIENTED_EDGE('',*,*,#3440,.F.);
#4277=ORIENTED_EDGE('',*,*,#3441,.T.);
#4278=ORIENTED_EDGE('',*,*,#3420,.F.);
#4279=ORIENTED_EDGE('',*,*,#3441,.F.);
#4280=ORIENTED_EDGE('',*,*,#3442,.F.);
#4281=ORIENTED_EDGE('',*,*,#3443,.T.);
#4282=ORIENTED_EDGE('',*,*,#3418,.F.);
#4283=ORIENTED_EDGE('',*,*,#3443,.F.);
#4284=ORIENTED_EDGE('',*,*,#3444,.F.);
#4285=ORIENTED_EDGE('',*,*,#3445,.T.);
#4286=ORIENTED_EDGE('',*,*,#3419,.F.);
#4287=ORIENTED_EDGE('',*,*,#3445,.F.);
#4288=ORIENTED_EDGE('',*,*,#3446,.F.);
#4289=ORIENTED_EDGE('',*,*,#3447,.T.);
#4290=ORIENTED_EDGE('',*,*,#3448,.F.);
#4291=ORIENTED_EDGE('',*,*,#3447,.F.);
#4292=ORIENTED_EDGE('',*,*,#3446,.T.);
#4293=ORIENTED_EDGE('',*,*,#3449,.F.);
#4294=ORIENTED_EDGE('',*,*,#3416,.F.);
#4295=ORIENTED_EDGE('',*,*,#3450,.T.);
#4296=ORIENTED_EDGE('',*,*,#3451,.T.);
#4297=ORIENTED_EDGE('',*,*,#3450,.F.);
#4298=ORIENTED_EDGE('',*,*,#3436,.T.);
#4299=ORIENTED_EDGE('',*,*,#3437,.T.);
#4300=ORIENTED_EDGE('',*,*,#3449,.T.);
#4301=ORIENTED_EDGE('',*,*,#3452,.T.);
#4302=ORIENTED_EDGE('',*,*,#3453,.T.);
#4303=ORIENTED_EDGE('',*,*,#3452,.F.);
#4304=ORIENTED_EDGE('',*,*,#3433,.T.);
#4305=ORIENTED_EDGE('',*,*,#3434,.T.);
#4306=ORIENTED_EDGE('',*,*,#3409,.T.);
#4307=ORIENTED_EDGE('',*,*,#3448,.T.);
#4308=ORIENTED_EDGE('',*,*,#3432,.T.);
#4309=ORIENTED_EDGE('',*,*,#3429,.T.);
#4310=ORIENTED_EDGE('',*,*,#3426,.T.);
#4311=ORIENTED_EDGE('',*,*,#3423,.T.);
#4312=ORIENTED_EDGE('',*,*,#3451,.F.);
#4313=ORIENTED_EDGE('',*,*,#3453,.F.);
#4314=ORIENTED_EDGE('',*,*,#3444,.T.);
#4315=ORIENTED_EDGE('',*,*,#3442,.T.);
#4316=ORIENTED_EDGE('',*,*,#3440,.T.);
#4317=ORIENTED_EDGE('',*,*,#3438,.T.);
#4318=ORIENTED_EDGE('',*,*,#3454,.F.);
#4319=ORIENTED_EDGE('',*,*,#3455,.T.);
#4320=ORIENTED_EDGE('',*,*,#3456,.T.);
#4321=ORIENTED_EDGE('',*,*,#3455,.F.);
#4322=ORIENTED_EDGE('',*,*,#3457,.F.);
#4323=ORIENTED_EDGE('',*,*,#3458,.T.);
#4324=ORIENTED_EDGE('',*,*,#3459,.T.);
#4325=ORIENTED_EDGE('',*,*,#3458,.F.);
#4326=ORIENTED_EDGE('',*,*,#3457,.T.);
#4327=ORIENTED_EDGE('',*,*,#3454,.T.);
#4328=ORIENTED_EDGE('',*,*,#3459,.F.);
#4329=ORIENTED_EDGE('',*,*,#3456,.F.);
#4330=ORIENTED_EDGE('',*,*,#3460,.F.);
#4331=ORIENTED_EDGE('',*,*,#3461,.T.);
#4332=ORIENTED_EDGE('',*,*,#3462,.F.);
#4333=ORIENTED_EDGE('',*,*,#3461,.F.);
#4334=ORIENTED_EDGE('',*,*,#3463,.F.);
#4335=ORIENTED_EDGE('',*,*,#3464,.T.);
#4336=ORIENTED_EDGE('',*,*,#3465,.F.);
#4337=ORIENTED_EDGE('',*,*,#3464,.F.);
#4338=ORIENTED_EDGE('',*,*,#3466,.F.);
#4339=ORIENTED_EDGE('',*,*,#3467,.T.);
#4340=ORIENTED_EDGE('',*,*,#3468,.F.);
#4341=ORIENTED_EDGE('',*,*,#3467,.F.);
#4342=ORIENTED_EDGE('',*,*,#3469,.F.);
#4343=ORIENTED_EDGE('',*,*,#3470,.T.);
#4344=ORIENTED_EDGE('',*,*,#3471,.F.);
#4345=ORIENTED_EDGE('',*,*,#3470,.F.);
#4346=ORIENTED_EDGE('',*,*,#3472,.F.);
#4347=ORIENTED_EDGE('',*,*,#3473,.T.);
#4348=ORIENTED_EDGE('',*,*,#3474,.T.);
#4349=ORIENTED_EDGE('',*,*,#3473,.F.);
#4350=ORIENTED_EDGE('',*,*,#3474,.F.);
#4351=ORIENTED_EDGE('',*,*,#3475,.F.);
#4352=ORIENTED_EDGE('',*,*,#3476,.F.);
#4353=ORIENTED_EDGE('',*,*,#3477,.T.);
#4354=ORIENTED_EDGE('',*,*,#3475,.T.);
#4355=ORIENTED_EDGE('',*,*,#3477,.F.);
#4356=ORIENTED_EDGE('',*,*,#3478,.F.);
#4357=ORIENTED_EDGE('',*,*,#3479,.T.);
#4358=ORIENTED_EDGE('',*,*,#3480,.T.);
#4359=ORIENTED_EDGE('',*,*,#3479,.F.);
#4360=ORIENTED_EDGE('',*,*,#3478,.T.);
#4361=ORIENTED_EDGE('',*,*,#3476,.T.);
#4362=ORIENTED_EDGE('',*,*,#3471,.T.);
#4363=ORIENTED_EDGE('',*,*,#3468,.T.);
#4364=ORIENTED_EDGE('',*,*,#3465,.T.);
#4365=ORIENTED_EDGE('',*,*,#3462,.T.);
#4366=ORIENTED_EDGE('',*,*,#3480,.F.);
#4367=ORIENTED_EDGE('',*,*,#3472,.T.);
#4368=ORIENTED_EDGE('',*,*,#3469,.T.);
#4369=ORIENTED_EDGE('',*,*,#3466,.T.);
#4370=ORIENTED_EDGE('',*,*,#3463,.T.);
#4371=ORIENTED_EDGE('',*,*,#3460,.T.);
#4372=ORIENTED_EDGE('',*,*,#3481,.F.);
#4373=ORIENTED_EDGE('',*,*,#3482,.F.);
#4374=ORIENTED_EDGE('',*,*,#3483,.F.);
#4375=ORIENTED_EDGE('',*,*,#3484,.F.);
#4376=ORIENTED_EDGE('',*,*,#3485,.F.);
#4377=ORIENTED_EDGE('',*,*,#3482,.T.);
#4378=ORIENTED_EDGE('',*,*,#3486,.F.);
#4379=ORIENTED_EDGE('',*,*,#3487,.T.);
#4380=ORIENTED_EDGE('',*,*,#3488,.F.);
#4381=ORIENTED_EDGE('',*,*,#3489,.F.);
#4382=ORIENTED_EDGE('',*,*,#3490,.F.);
#4383=ORIENTED_EDGE('',*,*,#3487,.F.);
#4384=ORIENTED_EDGE('',*,*,#3491,.F.);
#4385=ORIENTED_EDGE('',*,*,#3492,.T.);
#4386=ORIENTED_EDGE('',*,*,#3493,.F.);
#4387=ORIENTED_EDGE('',*,*,#3494,.F.);
#4388=ORIENTED_EDGE('',*,*,#3495,.F.);
#4389=ORIENTED_EDGE('',*,*,#3492,.F.);
#4390=ORIENTED_EDGE('',*,*,#3496,.F.);
#4391=ORIENTED_EDGE('',*,*,#3497,.T.);
#4392=ORIENTED_EDGE('',*,*,#3498,.F.);
#4393=ORIENTED_EDGE('',*,*,#3499,.F.);
#4394=ORIENTED_EDGE('',*,*,#3500,.F.);
#4395=ORIENTED_EDGE('',*,*,#3497,.F.);
#4396=ORIENTED_EDGE('',*,*,#3501,.F.);
#4397=ORIENTED_EDGE('',*,*,#3502,.T.);
#4398=ORIENTED_EDGE('',*,*,#3503,.T.);
#4399=ORIENTED_EDGE('',*,*,#3483,.T.);
#4400=ORIENTED_EDGE('',*,*,#3481,.T.);
#4401=ORIENTED_EDGE('',*,*,#3485,.T.);
#4402=ORIENTED_EDGE('',*,*,#3504,.T.);
#4403=ORIENTED_EDGE('',*,*,#3498,.T.);
#4404=ORIENTED_EDGE('',*,*,#3500,.T.);
#4405=ORIENTED_EDGE('',*,*,#3496,.T.);
#4406=ORIENTED_EDGE('',*,*,#3505,.T.);
#4407=ORIENTED_EDGE('',*,*,#3493,.T.);
#4408=ORIENTED_EDGE('',*,*,#3495,.T.);
#4409=ORIENTED_EDGE('',*,*,#3491,.T.);
#4410=ORIENTED_EDGE('',*,*,#3506,.T.);
#4411=ORIENTED_EDGE('',*,*,#3488,.T.);
#4412=ORIENTED_EDGE('',*,*,#3490,.T.);
#4413=ORIENTED_EDGE('',*,*,#3486,.T.);
#4414=ORIENTED_EDGE('',*,*,#3507,.T.);
#4415=ORIENTED_EDGE('',*,*,#3502,.F.);
#4416=ORIENTED_EDGE('',*,*,#3508,.T.);
#4417=ORIENTED_EDGE('',*,*,#3507,.F.);
#4418=ORIENTED_EDGE('',*,*,#3489,.T.);
#4419=ORIENTED_EDGE('',*,*,#3506,.F.);
#4420=ORIENTED_EDGE('',*,*,#3494,.T.);
#4421=ORIENTED_EDGE('',*,*,#3505,.F.);
#4422=ORIENTED_EDGE('',*,*,#3499,.T.);
#4423=ORIENTED_EDGE('',*,*,#3504,.F.);
#4424=ORIENTED_EDGE('',*,*,#3484,.T.);
#4425=ORIENTED_EDGE('',*,*,#3503,.F.);
#4426=ORIENTED_EDGE('',*,*,#3509,.T.);
#4427=ORIENTED_EDGE('',*,*,#3510,.T.);
#4428=ORIENTED_EDGE('',*,*,#3511,.T.);
#4429=ORIENTED_EDGE('',*,*,#3512,.T.);
#4430=ORIENTED_EDGE('',*,*,#3513,.F.);
#4431=ORIENTED_EDGE('',*,*,#3514,.T.);
#4432=ORIENTED_EDGE('',*,*,#3515,.F.);
#4433=ORIENTED_EDGE('',*,*,#3514,.F.);
#4434=ORIENTED_EDGE('',*,*,#3513,.T.);
#4435=ORIENTED_EDGE('',*,*,#3516,.F.);
#4436=ORIENTED_EDGE('',*,*,#3517,.T.);
#4437=ORIENTED_EDGE('',*,*,#3518,.F.);
#4438=ORIENTED_EDGE('',*,*,#3517,.F.);
#4439=ORIENTED_EDGE('',*,*,#3516,.T.);
#4440=ORIENTED_EDGE('',*,*,#3519,.F.);
#4441=ORIENTED_EDGE('',*,*,#3520,.T.);
#4442=ORIENTED_EDGE('',*,*,#3521,.F.);
#4443=ORIENTED_EDGE('',*,*,#3520,.F.);
#4444=ORIENTED_EDGE('',*,*,#3519,.T.);
#4445=ORIENTED_EDGE('',*,*,#3522,.F.);
#4446=ORIENTED_EDGE('',*,*,#3523,.T.);
#4447=ORIENTED_EDGE('',*,*,#3524,.F.);
#4448=ORIENTED_EDGE('',*,*,#3523,.F.);
#4449=ORIENTED_EDGE('',*,*,#3522,.T.);
#4450=ORIENTED_EDGE('',*,*,#3525,.F.);
#4451=ORIENTED_EDGE('',*,*,#3526,.F.);
#4452=ORIENTED_EDGE('',*,*,#3527,.T.);
#4453=ORIENTED_EDGE('',*,*,#3528,.F.);
#4454=ORIENTED_EDGE('',*,*,#3529,.F.);
#4455=ORIENTED_EDGE('',*,*,#3527,.F.);
#4456=ORIENTED_EDGE('',*,*,#3530,.F.);
#4457=ORIENTED_EDGE('',*,*,#3531,.T.);
#4458=ORIENTED_EDGE('',*,*,#3509,.F.);
#4459=ORIENTED_EDGE('',*,*,#3531,.F.);
#4460=ORIENTED_EDGE('',*,*,#3532,.F.);
#4461=ORIENTED_EDGE('',*,*,#3533,.T.);
#4462=ORIENTED_EDGE('',*,*,#3512,.F.);
#4463=ORIENTED_EDGE('',*,*,#3533,.F.);
#4464=ORIENTED_EDGE('',*,*,#3534,.F.);
#4465=ORIENTED_EDGE('',*,*,#3535,.T.);
#4466=ORIENTED_EDGE('',*,*,#3510,.F.);
#4467=ORIENTED_EDGE('',*,*,#3535,.F.);
#4468=ORIENTED_EDGE('',*,*,#3536,.F.);
#4469=ORIENTED_EDGE('',*,*,#3537,.T.);
#4470=ORIENTED_EDGE('',*,*,#3511,.F.);
#4471=ORIENTED_EDGE('',*,*,#3537,.F.);
#4472=ORIENTED_EDGE('',*,*,#3538,.F.);
#4473=ORIENTED_EDGE('',*,*,#3539,.T.);
#4474=ORIENTED_EDGE('',*,*,#3540,.F.);
#4475=ORIENTED_EDGE('',*,*,#3539,.F.);
#4476=ORIENTED_EDGE('',*,*,#3538,.T.);
#4477=ORIENTED_EDGE('',*,*,#3541,.F.);
#4478=ORIENTED_EDGE('',*,*,#3508,.F.);
#4479=ORIENTED_EDGE('',*,*,#3542,.T.);
#4480=ORIENTED_EDGE('',*,*,#3543,.T.);
#4481=ORIENTED_EDGE('',*,*,#3542,.F.);
#4482=ORIENTED_EDGE('',*,*,#3528,.T.);
#4483=ORIENTED_EDGE('',*,*,#3529,.T.);
#4484=ORIENTED_EDGE('',*,*,#3541,.T.);
#4485=ORIENTED_EDGE('',*,*,#3544,.T.);
#4486=ORIENTED_EDGE('',*,*,#3545,.T.);
#4487=ORIENTED_EDGE('',*,*,#3544,.F.);
#4488=ORIENTED_EDGE('',*,*,#3525,.T.);
#4489=ORIENTED_EDGE('',*,*,#3526,.T.);
#4490=ORIENTED_EDGE('',*,*,#3501,.T.);
#4491=ORIENTED_EDGE('',*,*,#3540,.T.);
#4492=ORIENTED_EDGE('',*,*,#3524,.T.);
#4493=ORIENTED_EDGE('',*,*,#3521,.T.);
#4494=ORIENTED_EDGE('',*,*,#3518,.T.);
#4495=ORIENTED_EDGE('',*,*,#3515,.T.);
#4496=ORIENTED_EDGE('',*,*,#3543,.F.);
#4497=ORIENTED_EDGE('',*,*,#3545,.F.);
#4498=ORIENTED_EDGE('',*,*,#3536,.T.);
#4499=ORIENTED_EDGE('',*,*,#3534,.T.);
#4500=ORIENTED_EDGE('',*,*,#3532,.T.);
#4501=ORIENTED_EDGE('',*,*,#3530,.T.);
#4502=ORIENTED_EDGE('',*,*,#3546,.F.);
#4503=ORIENTED_EDGE('',*,*,#3547,.T.);
#4504=ORIENTED_EDGE('',*,*,#3548,.F.);
#4505=ORIENTED_EDGE('',*,*,#3547,.F.);
#4506=ORIENTED_EDGE('',*,*,#3549,.F.);
#4507=ORIENTED_EDGE('',*,*,#3550,.T.);
#4508=ORIENTED_EDGE('',*,*,#3551,.F.);
#4509=ORIENTED_EDGE('',*,*,#3550,.F.);
#4510=ORIENTED_EDGE('',*,*,#3552,.F.);
#4511=ORIENTED_EDGE('',*,*,#3553,.T.);
#4512=ORIENTED_EDGE('',*,*,#3554,.F.);
#4513=ORIENTED_EDGE('',*,*,#3553,.F.);
#4514=ORIENTED_EDGE('',*,*,#3555,.F.);
#4515=ORIENTED_EDGE('',*,*,#3556,.T.);
#4516=ORIENTED_EDGE('',*,*,#3557,.F.);
#4517=ORIENTED_EDGE('',*,*,#3556,.F.);
#4518=ORIENTED_EDGE('',*,*,#3558,.F.);
#4519=ORIENTED_EDGE('',*,*,#3559,.T.);
#4520=ORIENTED_EDGE('',*,*,#3560,.T.);
#4521=ORIENTED_EDGE('',*,*,#3559,.F.);
#4522=ORIENTED_EDGE('',*,*,#3560,.F.);
#4523=ORIENTED_EDGE('',*,*,#3561,.F.);
#4524=ORIENTED_EDGE('',*,*,#3562,.F.);
#4525=ORIENTED_EDGE('',*,*,#3563,.T.);
#4526=ORIENTED_EDGE('',*,*,#3561,.T.);
#4527=ORIENTED_EDGE('',*,*,#3563,.F.);
#4528=ORIENTED_EDGE('',*,*,#3564,.F.);
#4529=ORIENTED_EDGE('',*,*,#3565,.T.);
#4530=ORIENTED_EDGE('',*,*,#3566,.T.);
#4531=ORIENTED_EDGE('',*,*,#3565,.F.);
#4532=ORIENTED_EDGE('',*,*,#3564,.T.);
#4533=ORIENTED_EDGE('',*,*,#3562,.T.);
#4534=ORIENTED_EDGE('',*,*,#3557,.T.);
#4535=ORIENTED_EDGE('',*,*,#3554,.T.);
#4536=ORIENTED_EDGE('',*,*,#3551,.T.);
#4537=ORIENTED_EDGE('',*,*,#3548,.T.);
#4538=ORIENTED_EDGE('',*,*,#3566,.F.);
#4539=ORIENTED_EDGE('',*,*,#3558,.T.);
#4540=ORIENTED_EDGE('',*,*,#3555,.T.);
#4541=ORIENTED_EDGE('',*,*,#3552,.T.);
#4542=ORIENTED_EDGE('',*,*,#3549,.T.);
#4543=ORIENTED_EDGE('',*,*,#3546,.T.);
#4544=ORIENTED_EDGE('',*,*,#3567,.T.);
#4545=ORIENTED_EDGE('',*,*,#3568,.T.);
#4546=ORIENTED_EDGE('',*,*,#3569,.T.);
#4547=ORIENTED_EDGE('',*,*,#3570,.F.);
#4548=ORIENTED_EDGE('',*,*,#3571,.T.);
#4549=ORIENTED_EDGE('',*,*,#3572,.T.);
#4550=ORIENTED_EDGE('',*,*,#3573,.T.);
#4551=ORIENTED_EDGE('',*,*,#3568,.F.);
#4552=ORIENTED_EDGE('',*,*,#3574,.T.);
#4553=ORIENTED_EDGE('',*,*,#3575,.T.);
#4554=ORIENTED_EDGE('',*,*,#3576,.T.);
#4555=ORIENTED_EDGE('',*,*,#3572,.F.);
#4556=ORIENTED_EDGE('',*,*,#3577,.T.);
#4557=ORIENTED_EDGE('',*,*,#3578,.T.);
#4558=ORIENTED_EDGE('',*,*,#3579,.T.);
#4559=ORIENTED_EDGE('',*,*,#3575,.F.);
#4560=ORIENTED_EDGE('',*,*,#3580,.T.);
#4561=ORIENTED_EDGE('',*,*,#3581,.T.);
#4562=ORIENTED_EDGE('',*,*,#3582,.T.);
#4563=ORIENTED_EDGE('',*,*,#3578,.F.);
#4564=ORIENTED_EDGE('',*,*,#3583,.T.);
#4565=ORIENTED_EDGE('',*,*,#3570,.T.);
#4566=ORIENTED_EDGE('',*,*,#3584,.T.);
#4567=ORIENTED_EDGE('',*,*,#3581,.F.);
#4568=ORIENTED_EDGE('',*,*,#3583,.F.);
#4569=ORIENTED_EDGE('',*,*,#3580,.F.);
#4570=ORIENTED_EDGE('',*,*,#3577,.F.);
#4571=ORIENTED_EDGE('',*,*,#3574,.F.);
#4572=ORIENTED_EDGE('',*,*,#3571,.F.);
#4573=ORIENTED_EDGE('',*,*,#3567,.F.);
#4574=ORIENTED_EDGE('',*,*,#3584,.F.);
#4575=ORIENTED_EDGE('',*,*,#3569,.F.);
#4576=ORIENTED_EDGE('',*,*,#3573,.F.);
#4577=ORIENTED_EDGE('',*,*,#3576,.F.);
#4578=ORIENTED_EDGE('',*,*,#3579,.F.);
#4579=ORIENTED_EDGE('',*,*,#3582,.F.);
#4580=ORIENTED_EDGE('',*,*,#3585,.F.);
#4581=ORIENTED_EDGE('',*,*,#3586,.F.);
#4582=ORIENTED_EDGE('',*,*,#3587,.F.);
#4583=ORIENTED_EDGE('',*,*,#3588,.T.);
#4584=ORIENTED_EDGE('',*,*,#3586,.T.);
#4585=ORIENTED_EDGE('',*,*,#3588,.F.);
#4586=ORIENTED_EDGE('',*,*,#3589,.F.);
#4587=ORIENTED_EDGE('',*,*,#3590,.T.);
#4588=ORIENTED_EDGE('',*,*,#3587,.T.);
#4589=ORIENTED_EDGE('',*,*,#3590,.F.);
#4590=ORIENTED_EDGE('',*,*,#3591,.F.);
#4591=ORIENTED_EDGE('',*,*,#3592,.T.);
#4592=ORIENTED_EDGE('',*,*,#3589,.T.);
#4593=ORIENTED_EDGE('',*,*,#3592,.F.);
#4594=ORIENTED_EDGE('',*,*,#3591,.T.);
#4595=ORIENTED_EDGE('',*,*,#3593,.F.);
#4596=ORIENTED_EDGE('',*,*,#3594,.F.);
#4597=ORIENTED_EDGE('',*,*,#3595,.T.);
#4598=ORIENTED_EDGE('',*,*,#3593,.T.);
#4599=ORIENTED_EDGE('',*,*,#3595,.F.);
#4600=ORIENTED_EDGE('',*,*,#3585,.T.);
#4601=ORIENTED_EDGE('',*,*,#3596,.T.);
#4602=ORIENTED_EDGE('',*,*,#3594,.T.);
#4603=ORIENTED_EDGE('',*,*,#3596,.F.);
#4604=ORIENTED_EDGE('',*,*,#3597,.F.);
#4605=ORIENTED_EDGE('',*,*,#3598,.F.);
#4606=ORIENTED_EDGE('',*,*,#3599,.T.);
#4607=ORIENTED_EDGE('',*,*,#3600,.F.);
#4608=ORIENTED_EDGE('',*,*,#3601,.F.);
#4609=ORIENTED_EDGE('',*,*,#3599,.F.);
#4610=ORIENTED_EDGE('',*,*,#3600,.T.);
#4611=ORIENTED_EDGE('',*,*,#3601,.T.);
#4612=ORIENTED_EDGE('',*,*,#3602,.T.);
#4613=ORIENTED_EDGE('',*,*,#3603,.T.);
#4614=ORIENTED_EDGE('',*,*,#3602,.F.);
#4615=ORIENTED_EDGE('',*,*,#3604,.T.);
#4616=ORIENTED_EDGE('',*,*,#3605,.T.);
#4617=ORIENTED_EDGE('',*,*,#3606,.F.);
#4618=ORIENTED_EDGE('',*,*,#3605,.F.);
#4619=ORIENTED_EDGE('',*,*,#3606,.T.);
#4620=ORIENTED_EDGE('',*,*,#3607,.T.);
#4621=ORIENTED_EDGE('',*,*,#3608,.F.);
#4622=ORIENTED_EDGE('',*,*,#3607,.F.);
#4623=ORIENTED_EDGE('',*,*,#3603,.F.);
#4624=ORIENTED_EDGE('',*,*,#3608,.T.);
#4625=ORIENTED_EDGE('',*,*,#3609,.F.);
#4626=ORIENTED_EDGE('',*,*,#3610,.T.);
#4627=ORIENTED_EDGE('',*,*,#3597,.T.);
#4628=ORIENTED_EDGE('',*,*,#3598,.T.);
#4629=ORIENTED_EDGE('',*,*,#3610,.F.);
#4630=ORIENTED_EDGE('',*,*,#3609,.T.);
#4631=ORIENTED_EDGE('',*,*,#3611,.F.);
#4632=ORIENTED_EDGE('',*,*,#3611,.T.);
#4633=ORIENTED_EDGE('',*,*,#3612,.T.);
#4634=ORIENTED_EDGE('',*,*,#3604,.F.);
#4635=ORIENTED_EDGE('',*,*,#3612,.F.);
#4636=ORIENTED_EDGE('',*,*,#3613,.F.);
#4637=ORIENTED_EDGE('',*,*,#3614,.F.);
#4638=ORIENTED_EDGE('',*,*,#3615,.T.);
#4639=ORIENTED_EDGE('',*,*,#3616,.F.);
#4640=ORIENTED_EDGE('',*,*,#3617,.F.);
#4641=ORIENTED_EDGE('',*,*,#3615,.F.);
#4642=ORIENTED_EDGE('',*,*,#3618,.T.);
#4643=ORIENTED_EDGE('',*,*,#3619,.T.);
#4644=ORIENTED_EDGE('',*,*,#3616,.T.);
#4645=ORIENTED_EDGE('',*,*,#3617,.T.);
#4646=ORIENTED_EDGE('',*,*,#3619,.F.);
#4647=ORIENTED_EDGE('',*,*,#3620,.F.);
#4648=ORIENTED_EDGE('',*,*,#3621,.T.);
#4649=ORIENTED_EDGE('',*,*,#3622,.F.);
#4650=ORIENTED_EDGE('',*,*,#3623,.T.);
#4651=ORIENTED_EDGE('',*,*,#3620,.T.);
#4652=ORIENTED_EDGE('',*,*,#3623,.F.);
#4653=ORIENTED_EDGE('',*,*,#3624,.F.);
#4654=ORIENTED_EDGE('',*,*,#3625,.T.);
#4655=ORIENTED_EDGE('',*,*,#3622,.T.);
#4656=ORIENTED_EDGE('',*,*,#3625,.F.);
#4657=ORIENTED_EDGE('',*,*,#3626,.F.);
#4658=ORIENTED_EDGE('',*,*,#3627,.T.);
#4659=ORIENTED_EDGE('',*,*,#3624,.T.);
#4660=ORIENTED_EDGE('',*,*,#3627,.F.);
#4661=ORIENTED_EDGE('',*,*,#3626,.T.);
#4662=ORIENTED_EDGE('',*,*,#3618,.F.);
#4663=ORIENTED_EDGE('',*,*,#3613,.T.);
#4664=ORIENTED_EDGE('',*,*,#3614,.T.);
#4665=ORIENTED_EDGE('',*,*,#3628,.T.);
#4666=ORIENTED_EDGE('',*,*,#3621,.F.);
#4667=ORIENTED_EDGE('',*,*,#3628,.F.);
#4668=ORIENTED_EDGE('',*,*,#3629,.T.);
#4669=ORIENTED_EDGE('',*,*,#3629,.F.);
#4670=ORIENTED_EDGE('',*,*,#3630,.T.);
#4671=ORIENTED_EDGE('',*,*,#3630,.F.);
#4672=ORIENTED_EDGE('',*,*,#3631,.T.);
#4673=ORIENTED_EDGE('',*,*,#3631,.F.);
#4674=ORIENTED_EDGE('',*,*,#3632,.T.);
#4675=ORIENTED_EDGE('',*,*,#3632,.F.);
#4676=ORIENTED_EDGE('',*,*,#3633,.T.);
#4677=ORIENTED_EDGE('',*,*,#3633,.F.);
#4678=ORIENTED_EDGE('',*,*,#3634,.T.);
#4679=ORIENTED_EDGE('',*,*,#3634,.F.);
#4680=ORIENTED_EDGE('',*,*,#3635,.T.);
#4681=ORIENTED_EDGE('',*,*,#3635,.F.);
#4682=ORIENTED_EDGE('',*,*,#3636,.T.);
#4683=ORIENTED_EDGE('',*,*,#3636,.F.);
#4684=ORIENTED_EDGE('',*,*,#3637,.F.);
#4685=ORIENTED_EDGE('',*,*,#3638,.F.);
#4686=ORIENTED_EDGE('',*,*,#3639,.F.);
#4687=ORIENTED_EDGE('',*,*,#3640,.F.);
#4688=ORIENTED_EDGE('',*,*,#3639,.T.);
#4689=ORIENTED_EDGE('',*,*,#3641,.F.);
#4690=ORIENTED_EDGE('',*,*,#3642,.T.);
#4691=ORIENTED_EDGE('',*,*,#3643,.F.);
#4692=ORIENTED_EDGE('',*,*,#3644,.T.);
#4693=ORIENTED_EDGE('',*,*,#3645,.F.);
#4694=ORIENTED_EDGE('',*,*,#3646,.T.);
#4695=ORIENTED_EDGE('',*,*,#3647,.T.);
#4696=ORIENTED_EDGE('',*,*,#3648,.F.);
#4697=ORIENTED_EDGE('',*,*,#3647,.F.);
#4698=ORIENTED_EDGE('',*,*,#3649,.T.);
#4699=ORIENTED_EDGE('',*,*,#3650,.F.);
#4700=ORIENTED_EDGE('',*,*,#3651,.T.);
#4701=ORIENTED_EDGE('',*,*,#3652,.F.);
#4702=ORIENTED_EDGE('',*,*,#3653,.T.);
#4703=ORIENTED_EDGE('',*,*,#3654,.F.);
#4704=ORIENTED_EDGE('',*,*,#3655,.T.);
#4705=ORIENTED_EDGE('',*,*,#3656,.F.);
#4706=ORIENTED_EDGE('',*,*,#3657,.T.);
#4707=ORIENTED_EDGE('',*,*,#3658,.F.);
#4708=ORIENTED_EDGE('',*,*,#3638,.T.);
#4709=ORIENTED_EDGE('',*,*,#3659,.T.);
#4710=ORIENTED_EDGE('',*,*,#3660,.T.);
#4711=ORIENTED_EDGE('',*,*,#3641,.T.);
#4712=ORIENTED_EDGE('',*,*,#3661,.F.);
#4713=ORIENTED_EDGE('',*,*,#3662,.F.);
#4714=ORIENTED_EDGE('',*,*,#3642,.F.);
#4715=ORIENTED_EDGE('',*,*,#3660,.F.);
#4716=ORIENTED_EDGE('',*,*,#3662,.T.);
#4717=ORIENTED_EDGE('',*,*,#3663,.T.);
#4718=ORIENTED_EDGE('',*,*,#3664,.T.);
#4719=ORIENTED_EDGE('',*,*,#3643,.T.);
#4720=ORIENTED_EDGE('',*,*,#3665,.F.);
#4721=ORIENTED_EDGE('',*,*,#3666,.F.);
#4722=ORIENTED_EDGE('',*,*,#3644,.F.);
#4723=ORIENTED_EDGE('',*,*,#3664,.F.);
#4724=ORIENTED_EDGE('',*,*,#3666,.T.);
#4725=ORIENTED_EDGE('',*,*,#3667,.T.);
#4726=ORIENTED_EDGE('',*,*,#3668,.T.);
#4727=ORIENTED_EDGE('',*,*,#3645,.T.);
#4728=ORIENTED_EDGE('',*,*,#3669,.F.);
#4729=ORIENTED_EDGE('',*,*,#3670,.F.);
#4730=ORIENTED_EDGE('',*,*,#3649,.F.);
#4731=ORIENTED_EDGE('',*,*,#3646,.F.);
#4732=ORIENTED_EDGE('',*,*,#3668,.F.);
#4733=ORIENTED_EDGE('',*,*,#3671,.F.);
#4734=ORIENTED_EDGE('',*,*,#3670,.T.);
#4735=ORIENTED_EDGE('',*,*,#3672,.T.);
#4736=ORIENTED_EDGE('',*,*,#3673,.T.);
#4737=ORIENTED_EDGE('',*,*,#3650,.T.);
#4738=ORIENTED_EDGE('',*,*,#3674,.F.);
#4739=ORIENTED_EDGE('',*,*,#3675,.F.);
#4740=ORIENTED_EDGE('',*,*,#3651,.F.);
#4741=ORIENTED_EDGE('',*,*,#3673,.F.);
#4742=ORIENTED_EDGE('',*,*,#3675,.T.);
#4743=ORIENTED_EDGE('',*,*,#3676,.T.);
#4744=ORIENTED_EDGE('',*,*,#3677,.T.);
#4745=ORIENTED_EDGE('',*,*,#3652,.T.);
#4746=ORIENTED_EDGE('',*,*,#3678,.F.);
#4747=ORIENTED_EDGE('',*,*,#3679,.F.);
#4748=ORIENTED_EDGE('',*,*,#3653,.F.);
#4749=ORIENTED_EDGE('',*,*,#3677,.F.);
#4750=ORIENTED_EDGE('',*,*,#3679,.T.);
#4751=ORIENTED_EDGE('',*,*,#3680,.T.);
#4752=ORIENTED_EDGE('',*,*,#3681,.T.);
#4753=ORIENTED_EDGE('',*,*,#3654,.T.);
#4754=ORIENTED_EDGE('',*,*,#3655,.F.);
#4755=ORIENTED_EDGE('',*,*,#3681,.F.);
#4756=ORIENTED_EDGE('',*,*,#3682,.F.);
#4757=ORIENTED_EDGE('',*,*,#3683,.F.);
#4758=ORIENTED_EDGE('',*,*,#3684,.F.);
#4759=ORIENTED_EDGE('',*,*,#3685,.T.);
#4760=ORIENTED_EDGE('',*,*,#3671,.T.);
#4761=ORIENTED_EDGE('',*,*,#3667,.F.);
#4762=ORIENTED_EDGE('',*,*,#3665,.T.);
#4763=ORIENTED_EDGE('',*,*,#3663,.F.);
#4764=ORIENTED_EDGE('',*,*,#3661,.T.);
#4765=ORIENTED_EDGE('',*,*,#3659,.F.);
#4766=ORIENTED_EDGE('',*,*,#3637,.T.);
#4767=ORIENTED_EDGE('',*,*,#3686,.F.);
#4768=ORIENTED_EDGE('',*,*,#3687,.T.);
#4769=ORIENTED_EDGE('',*,*,#3688,.F.);
#4770=ORIENTED_EDGE('',*,*,#3682,.T.);
#4771=ORIENTED_EDGE('',*,*,#3680,.F.);
#4772=ORIENTED_EDGE('',*,*,#3678,.T.);
#4773=ORIENTED_EDGE('',*,*,#3676,.F.);
#4774=ORIENTED_EDGE('',*,*,#3674,.T.);
#4775=ORIENTED_EDGE('',*,*,#3672,.F.);
#4776=ORIENTED_EDGE('',*,*,#3669,.T.);
#4777=ORIENTED_EDGE('',*,*,#3685,.F.);
#4778=ORIENTED_EDGE('',*,*,#3640,.T.);
#4779=ORIENTED_EDGE('',*,*,#3658,.T.);
#4780=ORIENTED_EDGE('',*,*,#3689,.T.);
#4781=ORIENTED_EDGE('',*,*,#3686,.T.);
#4782=ORIENTED_EDGE('',*,*,#3657,.F.);
#4783=ORIENTED_EDGE('',*,*,#3690,.F.);
#4784=ORIENTED_EDGE('',*,*,#3687,.F.);
#4785=ORIENTED_EDGE('',*,*,#3689,.F.);
#4786=ORIENTED_EDGE('',*,*,#3648,.T.);
#4787=ORIENTED_EDGE('',*,*,#3684,.T.);
#4788=ORIENTED_EDGE('',*,*,#3683,.T.);
#4789=ORIENTED_EDGE('',*,*,#3688,.T.);
#4790=ORIENTED_EDGE('',*,*,#3690,.T.);
#4791=ORIENTED_EDGE('',*,*,#3656,.T.);
#4792=ORIENTED_EDGE('',*,*,#3691,.F.);
#4793=ORIENTED_EDGE('',*,*,#3692,.T.);
#4794=ORIENTED_EDGE('',*,*,#3693,.F.);
#4795=ORIENTED_EDGE('',*,*,#3694,.T.);
#4796=ORIENTED_EDGE('',*,*,#3691,.T.);
#4797=ORIENTED_EDGE('',*,*,#3694,.F.);
#4798=ORIENTED_EDGE('',*,*,#3693,.T.);
#4799=ORIENTED_EDGE('',*,*,#3695,.F.);
#4800=ORIENTED_EDGE('',*,*,#3695,.T.);
#4801=ORIENTED_EDGE('',*,*,#3696,.T.);
#4802=ORIENTED_EDGE('',*,*,#3692,.F.);
#4803=ORIENTED_EDGE('',*,*,#3696,.F.);
#4804=ORIENTED_EDGE('',*,*,#3697,.F.);
#4805=ORIENTED_EDGE('',*,*,#3698,.T.);
#4806=ORIENTED_EDGE('',*,*,#3699,.F.);
#4807=ORIENTED_EDGE('',*,*,#3700,.T.);
#4808=ORIENTED_EDGE('',*,*,#3697,.T.);
#4809=ORIENTED_EDGE('',*,*,#3700,.F.);
#4810=ORIENTED_EDGE('',*,*,#3699,.T.);
#4811=ORIENTED_EDGE('',*,*,#3701,.F.);
#4812=ORIENTED_EDGE('',*,*,#3701,.T.);
#4813=ORIENTED_EDGE('',*,*,#3702,.T.);
#4814=ORIENTED_EDGE('',*,*,#3698,.F.);
#4815=ORIENTED_EDGE('',*,*,#3702,.F.);
#4816=ORIENTED_EDGE('',*,*,#3703,.F.);
#4817=ORIENTED_EDGE('',*,*,#3704,.T.);
#4818=ORIENTED_EDGE('',*,*,#3705,.F.);
#4819=ORIENTED_EDGE('',*,*,#3704,.F.);
#4820=ORIENTED_EDGE('',*,*,#3703,.T.);
#4821=ORIENTED_EDGE('',*,*,#3706,.F.);
#4822=ORIENTED_EDGE('',*,*,#3707,.T.);
#4823=ORIENTED_EDGE('',*,*,#3708,.F.);
#4824=ORIENTED_EDGE('',*,*,#3707,.F.);
#4825=ORIENTED_EDGE('',*,*,#3709,.F.);
#4826=ORIENTED_EDGE('',*,*,#3710,.T.);
#4827=ORIENTED_EDGE('',*,*,#3711,.F.);
#4828=ORIENTED_EDGE('',*,*,#3712,.F.);
#4829=ORIENTED_EDGE('',*,*,#3709,.T.);
#4830=ORIENTED_EDGE('',*,*,#3713,.F.);
#4831=ORIENTED_EDGE('',*,*,#3714,.F.);
#4832=ORIENTED_EDGE('',*,*,#3715,.F.);
#4833=ORIENTED_EDGE('',*,*,#3712,.T.);
#4834=ORIENTED_EDGE('',*,*,#3716,.T.);
#4835=ORIENTED_EDGE('',*,*,#3717,.T.);
#4836=ORIENTED_EDGE('',*,*,#3713,.T.);
#4837=ORIENTED_EDGE('',*,*,#3708,.T.);
#4838=ORIENTED_EDGE('',*,*,#3718,.F.);
#4839=ORIENTED_EDGE('',*,*,#3711,.T.);
#4840=ORIENTED_EDGE('',*,*,#3719,.F.);
#4841=ORIENTED_EDGE('',*,*,#3720,.F.);
#4842=ORIENTED_EDGE('',*,*,#3716,.F.);
#4843=ORIENTED_EDGE('',*,*,#3720,.T.);
#4844=ORIENTED_EDGE('',*,*,#3721,.T.);
#4845=ORIENTED_EDGE('',*,*,#3714,.T.);
#4846=ORIENTED_EDGE('',*,*,#3717,.F.);
#4847=ORIENTED_EDGE('',*,*,#3715,.T.);
#4848=ORIENTED_EDGE('',*,*,#3721,.F.);
#4849=ORIENTED_EDGE('',*,*,#3719,.T.);
#4850=ORIENTED_EDGE('',*,*,#3710,.F.);
#4851=ORIENTED_EDGE('',*,*,#3706,.T.);
#4852=ORIENTED_EDGE('',*,*,#3722,.T.);
#4853=ORIENTED_EDGE('',*,*,#3723,.F.);
#4854=ORIENTED_EDGE('',*,*,#3724,.F.);
#4855=ORIENTED_EDGE('',*,*,#3722,.F.);
#4856=ORIENTED_EDGE('',*,*,#3725,.T.);
#4857=ORIENTED_EDGE('',*,*,#3723,.T.);
#4858=ORIENTED_EDGE('',*,*,#3725,.F.);
#4859=ORIENTED_EDGE('',*,*,#3724,.T.);
#4860=ORIENTED_EDGE('',*,*,#3726,.T.);
#4861=ORIENTED_EDGE('',*,*,#3727,.T.);
#4862=ORIENTED_EDGE('',*,*,#3726,.F.);
#4863=ORIENTED_EDGE('',*,*,#3728,.F.);
#4864=ORIENTED_EDGE('',*,*,#3729,.T.);
#4865=ORIENTED_EDGE('',*,*,#3718,.T.);
#4866=ORIENTED_EDGE('',*,*,#3729,.F.);
#4867=ORIENTED_EDGE('',*,*,#3728,.T.);
#4868=ORIENTED_EDGE('',*,*,#3705,.T.);
#4869=ORIENTED_EDGE('',*,*,#3727,.F.);
#4870=ORIENTED_EDGE('',*,*,#3730,.F.);
#4871=ORIENTED_EDGE('',*,*,#3731,.T.);
#4872=ORIENTED_EDGE('',*,*,#3732,.T.);
#4873=ORIENTED_EDGE('',*,*,#3731,.F.);
#4874=ORIENTED_EDGE('',*,*,#3733,.F.);
#4875=ORIENTED_EDGE('',*,*,#3734,.T.);
#4876=ORIENTED_EDGE('',*,*,#3735,.T.);
#4877=ORIENTED_EDGE('',*,*,#3734,.F.);
#4878=ORIENTED_EDGE('',*,*,#3733,.T.);
#4879=ORIENTED_EDGE('',*,*,#3730,.T.);
#4880=ORIENTED_EDGE('',*,*,#3735,.F.);
#4881=ORIENTED_EDGE('',*,*,#3732,.F.);
#4882=ORIENTED_EDGE('',*,*,#3736,.F.);
#4883=ORIENTED_EDGE('',*,*,#3737,.T.);
#4884=ORIENTED_EDGE('',*,*,#3738,.T.);
#4885=ORIENTED_EDGE('',*,*,#3737,.F.);
#4886=ORIENTED_EDGE('',*,*,#3739,.F.);
#4887=ORIENTED_EDGE('',*,*,#3740,.T.);
#4888=ORIENTED_EDGE('',*,*,#3741,.T.);
#4889=ORIENTED_EDGE('',*,*,#3740,.F.);
#4890=ORIENTED_EDGE('',*,*,#3739,.T.);
#4891=ORIENTED_EDGE('',*,*,#3736,.T.);
#4892=ORIENTED_EDGE('',*,*,#3741,.F.);
#4893=ORIENTED_EDGE('',*,*,#3738,.F.);
#4894=ORIENTED_EDGE('',*,*,#3742,.F.);
#4895=ORIENTED_EDGE('',*,*,#3743,.T.);
#4896=ORIENTED_EDGE('',*,*,#3744,.F.);
#4897=ORIENTED_EDGE('',*,*,#3745,.F.);
#4898=ORIENTED_EDGE('',*,*,#3746,.F.);
#4899=ORIENTED_EDGE('',*,*,#3747,.T.);
#4900=ORIENTED_EDGE('',*,*,#3748,.F.);
#4901=ORIENTED_EDGE('',*,*,#3749,.F.);
#4902=ORIENTED_EDGE('',*,*,#3747,.F.);
#4903=ORIENTED_EDGE('',*,*,#3750,.F.);
#4904=ORIENTED_EDGE('',*,*,#3743,.F.);
#4905=ORIENTED_EDGE('',*,*,#3751,.F.);
#4906=ORIENTED_EDGE('',*,*,#3745,.T.);
#4907=ORIENTED_EDGE('',*,*,#3752,.F.);
#4908=ORIENTED_EDGE('',*,*,#3753,.T.);
#4909=ORIENTED_EDGE('',*,*,#3754,.T.);
#4910=ORIENTED_EDGE('',*,*,#3753,.F.);
#4911=ORIENTED_EDGE('',*,*,#3750,.T.);
#4912=ORIENTED_EDGE('',*,*,#3746,.T.);
#4913=ORIENTED_EDGE('',*,*,#3751,.T.);
#4914=ORIENTED_EDGE('',*,*,#3744,.T.);
#4915=ORIENTED_EDGE('',*,*,#3742,.T.);
#4916=ORIENTED_EDGE('',*,*,#3755,.F.);
#4917=ORIENTED_EDGE('',*,*,#3756,.T.);
#4918=ORIENTED_EDGE('',*,*,#3757,.T.);
#4919=ORIENTED_EDGE('',*,*,#3756,.F.);
#4920=ORIENTED_EDGE('',*,*,#3748,.T.);
#4921=ORIENTED_EDGE('',*,*,#3749,.T.);
#4922=ORIENTED_EDGE('',*,*,#3755,.T.);
#4923=ORIENTED_EDGE('',*,*,#3752,.T.);
#4924=ORIENTED_EDGE('',*,*,#3757,.F.);
#4925=ORIENTED_EDGE('',*,*,#3754,.F.);
#4926=ORIENTED_EDGE('',*,*,#3758,.F.);
#4927=ORIENTED_EDGE('',*,*,#3759,.T.);
#4928=ORIENTED_EDGE('',*,*,#3760,.F.);
#4929=ORIENTED_EDGE('',*,*,#3761,.F.);
#4930=ORIENTED_EDGE('',*,*,#3762,.F.);
#4931=ORIENTED_EDGE('',*,*,#3763,.T.);
#4932=ORIENTED_EDGE('',*,*,#3764,.F.);
#4933=ORIENTED_EDGE('',*,*,#3765,.F.);
#4934=ORIENTED_EDGE('',*,*,#3763,.F.);
#4935=ORIENTED_EDGE('',*,*,#3766,.F.);
#4936=ORIENTED_EDGE('',*,*,#3759,.F.);
#4937=ORIENTED_EDGE('',*,*,#3767,.F.);
#4938=ORIENTED_EDGE('',*,*,#3761,.T.);
#4939=ORIENTED_EDGE('',*,*,#3768,.F.);
#4940=ORIENTED_EDGE('',*,*,#3769,.T.);
#4941=ORIENTED_EDGE('',*,*,#3770,.T.);
#4942=ORIENTED_EDGE('',*,*,#3769,.F.);
#4943=ORIENTED_EDGE('',*,*,#3766,.T.);
#4944=ORIENTED_EDGE('',*,*,#3762,.T.);
#4945=ORIENTED_EDGE('',*,*,#3767,.T.);
#4946=ORIENTED_EDGE('',*,*,#3760,.T.);
#4947=ORIENTED_EDGE('',*,*,#3758,.T.);
#4948=ORIENTED_EDGE('',*,*,#3771,.F.);
#4949=ORIENTED_EDGE('',*,*,#3772,.T.);
#4950=ORIENTED_EDGE('',*,*,#3773,.T.);
#4951=ORIENTED_EDGE('',*,*,#3772,.F.);
#4952=ORIENTED_EDGE('',*,*,#3764,.T.);
#4953=ORIENTED_EDGE('',*,*,#3765,.T.);
#4954=ORIENTED_EDGE('',*,*,#3771,.T.);
#4955=ORIENTED_EDGE('',*,*,#3768,.T.);
#4956=ORIENTED_EDGE('',*,*,#3773,.F.);
#4957=ORIENTED_EDGE('',*,*,#3770,.F.);
#4958=ORIENTED_EDGE('',*,*,#3774,.F.);
#4959=ORIENTED_EDGE('',*,*,#3775,.T.);
#4960=ORIENTED_EDGE('',*,*,#3776,.T.);
#4961=ORIENTED_EDGE('',*,*,#3775,.F.);
#4962=ORIENTED_EDGE('',*,*,#3777,.F.);
#4963=ORIENTED_EDGE('',*,*,#3778,.T.);
#4964=ORIENTED_EDGE('',*,*,#3779,.T.);
#4965=ORIENTED_EDGE('',*,*,#3778,.F.);
#4966=ORIENTED_EDGE('',*,*,#3777,.T.);
#4967=ORIENTED_EDGE('',*,*,#3774,.T.);
#4968=ORIENTED_EDGE('',*,*,#3779,.F.);
#4969=ORIENTED_EDGE('',*,*,#3776,.F.);
#4970=ORIENTED_EDGE('',*,*,#3780,.F.);
#4971=ORIENTED_EDGE('',*,*,#3781,.T.);
#4972=ORIENTED_EDGE('',*,*,#3782,.F.);
#4973=ORIENTED_EDGE('',*,*,#3781,.F.);
#4974=ORIENTED_EDGE('',*,*,#3780,.T.);
#4975=ORIENTED_EDGE('',*,*,#3783,.F.);
#4976=ORIENTED_EDGE('',*,*,#3784,.T.);
#4977=ORIENTED_EDGE('',*,*,#3785,.T.);
#4978=ORIENTED_EDGE('',*,*,#3784,.F.);
#4979=ORIENTED_EDGE('',*,*,#3785,.F.);
#4980=ORIENTED_EDGE('',*,*,#3786,.T.);
#4981=ORIENTED_EDGE('',*,*,#3787,.F.);
#4982=ORIENTED_EDGE('',*,*,#3788,.F.);
#4983=ORIENTED_EDGE('',*,*,#3789,.F.);
#4984=ORIENTED_EDGE('',*,*,#3786,.F.);
#4985=ORIENTED_EDGE('',*,*,#3790,.T.);
#4986=ORIENTED_EDGE('',*,*,#3788,.T.);
#4987=ORIENTED_EDGE('',*,*,#3790,.F.);
#4988=ORIENTED_EDGE('',*,*,#3789,.T.);
#4989=ORIENTED_EDGE('',*,*,#3791,.T.);
#4990=ORIENTED_EDGE('',*,*,#3792,.T.);
#4991=ORIENTED_EDGE('',*,*,#3791,.F.);
#4992=ORIENTED_EDGE('',*,*,#3793,.F.);
#4993=ORIENTED_EDGE('',*,*,#3794,.T.);
#4994=ORIENTED_EDGE('',*,*,#3787,.T.);
#4995=ORIENTED_EDGE('',*,*,#3794,.F.);
#4996=ORIENTED_EDGE('',*,*,#3793,.T.);
#4997=ORIENTED_EDGE('',*,*,#3782,.T.);
#4998=ORIENTED_EDGE('',*,*,#3792,.F.);
#4999=ORIENTED_EDGE('',*,*,#3783,.T.);
#5000=ORIENTED_EDGE('',*,*,#3795,.F.);
#5001=ORIENTED_EDGE('',*,*,#3796,.T.);
#5002=ORIENTED_EDGE('',*,*,#3797,.T.);
#5003=ORIENTED_EDGE('',*,*,#3796,.F.);
#5004=ORIENTED_EDGE('',*,*,#3798,.F.);
#5005=ORIENTED_EDGE('',*,*,#3799,.T.);
#5006=ORIENTED_EDGE('',*,*,#3800,.T.);
#5007=ORIENTED_EDGE('',*,*,#3799,.F.);
#5008=ORIENTED_EDGE('',*,*,#3798,.T.);
#5009=ORIENTED_EDGE('',*,*,#3795,.T.);
#5010=ORIENTED_EDGE('',*,*,#3800,.F.);
#5011=ORIENTED_EDGE('',*,*,#3797,.F.);
#5012=ORIENTED_EDGE('',*,*,#3801,.F.);
#5013=ORIENTED_EDGE('',*,*,#3802,.T.);
#5014=ORIENTED_EDGE('',*,*,#3803,.T.);
#5015=ORIENTED_EDGE('',*,*,#3802,.F.);
#5016=ORIENTED_EDGE('',*,*,#3804,.F.);
#5017=ORIENTED_EDGE('',*,*,#3805,.T.);
#5018=ORIENTED_EDGE('',*,*,#3806,.T.);
#5019=ORIENTED_EDGE('',*,*,#3805,.F.);
#5020=ORIENTED_EDGE('',*,*,#3804,.T.);
#5021=ORIENTED_EDGE('',*,*,#3801,.T.);
#5022=ORIENTED_EDGE('',*,*,#3806,.F.);
#5023=ORIENTED_EDGE('',*,*,#3803,.F.);
#5024=ORIENTED_EDGE('',*,*,#3807,.F.);
#5025=ORIENTED_EDGE('',*,*,#3808,.T.);
#5026=ORIENTED_EDGE('',*,*,#3809,.T.);
#5027=ORIENTED_EDGE('',*,*,#3808,.F.);
#5028=ORIENTED_EDGE('',*,*,#3810,.F.);
#5029=ORIENTED_EDGE('',*,*,#3811,.T.);
#5030=ORIENTED_EDGE('',*,*,#3812,.T.);
#5031=ORIENTED_EDGE('',*,*,#3811,.F.);
#5032=ORIENTED_EDGE('',*,*,#3810,.T.);
#5033=ORIENTED_EDGE('',*,*,#3807,.T.);
#5034=ORIENTED_EDGE('',*,*,#3812,.F.);
#5035=ORIENTED_EDGE('',*,*,#3809,.F.);
#5036=ORIENTED_EDGE('',*,*,#3813,.F.);
#5037=ORIENTED_EDGE('',*,*,#3814,.T.);
#5038=ORIENTED_EDGE('',*,*,#3815,.T.);
#5039=ORIENTED_EDGE('',*,*,#3814,.F.);
#5040=ORIENTED_EDGE('',*,*,#3816,.F.);
#5041=ORIENTED_EDGE('',*,*,#3817,.T.);
#5042=ORIENTED_EDGE('',*,*,#3818,.T.);
#5043=ORIENTED_EDGE('',*,*,#3817,.F.);
#5044=ORIENTED_EDGE('',*,*,#3816,.T.);
#5045=ORIENTED_EDGE('',*,*,#3813,.T.);
#5046=ORIENTED_EDGE('',*,*,#3818,.F.);
#5047=ORIENTED_EDGE('',*,*,#3815,.F.);
#5048=ORIENTED_EDGE('',*,*,#3819,.F.);
#5049=ORIENTED_EDGE('',*,*,#3820,.T.);
#5050=ORIENTED_EDGE('',*,*,#3821,.T.);
#5051=ORIENTED_EDGE('',*,*,#3822,.F.);
#5052=ORIENTED_EDGE('',*,*,#3823,.F.);
#5053=ORIENTED_EDGE('',*,*,#3824,.T.);
#5054=ORIENTED_EDGE('',*,*,#3825,.T.);
#5055=ORIENTED_EDGE('',*,*,#3820,.F.);
#5056=ORIENTED_EDGE('',*,*,#3826,.F.);
#5057=ORIENTED_EDGE('',*,*,#3827,.T.);
#5058=ORIENTED_EDGE('',*,*,#3828,.T.);
#5059=ORIENTED_EDGE('',*,*,#3824,.F.);
#5060=ORIENTED_EDGE('',*,*,#3829,.F.);
#5061=ORIENTED_EDGE('',*,*,#3830,.T.);
#5062=ORIENTED_EDGE('',*,*,#3831,.T.);
#5063=ORIENTED_EDGE('',*,*,#3827,.F.);
#5064=ORIENTED_EDGE('',*,*,#3832,.F.);
#5065=ORIENTED_EDGE('',*,*,#3833,.T.);
#5066=ORIENTED_EDGE('',*,*,#3834,.T.);
#5067=ORIENTED_EDGE('',*,*,#3830,.F.);
#5068=ORIENTED_EDGE('',*,*,#3835,.F.);
#5069=ORIENTED_EDGE('',*,*,#3822,.T.);
#5070=ORIENTED_EDGE('',*,*,#3836,.T.);
#5071=ORIENTED_EDGE('',*,*,#3833,.F.);
#5072=ORIENTED_EDGE('',*,*,#3836,.F.);
#5073=ORIENTED_EDGE('',*,*,#3821,.F.);
#5074=ORIENTED_EDGE('',*,*,#3825,.F.);
#5075=ORIENTED_EDGE('',*,*,#3828,.F.);
#5076=ORIENTED_EDGE('',*,*,#3831,.F.);
#5077=ORIENTED_EDGE('',*,*,#3834,.F.);
#5078=ORIENTED_EDGE('',*,*,#3837,.F.);
#5079=ORIENTED_EDGE('',*,*,#3819,.T.);
#5080=ORIENTED_EDGE('',*,*,#3835,.T.);
#5081=ORIENTED_EDGE('',*,*,#3832,.T.);
#5082=ORIENTED_EDGE('',*,*,#3829,.T.);
#5083=ORIENTED_EDGE('',*,*,#3826,.T.);
#5084=ORIENTED_EDGE('',*,*,#3823,.T.);
#5085=ORIENTED_EDGE('',*,*,#3838,.F.);
#5086=ORIENTED_EDGE('',*,*,#3839,.T.);
#5087=ORIENTED_EDGE('',*,*,#3837,.T.);
#5088=ORIENTED_EDGE('',*,*,#3839,.F.);
#5089=ORIENTED_EDGE('',*,*,#3840,.F.);
#5090=ORIENTED_EDGE('',*,*,#3841,.T.);
#5091=ORIENTED_EDGE('',*,*,#3838,.T.);
#5092=ORIENTED_EDGE('',*,*,#3841,.F.);
#5093=ORIENTED_EDGE('',*,*,#3842,.F.);
#5094=ORIENTED_EDGE('',*,*,#3843,.T.);
#5095=ORIENTED_EDGE('',*,*,#3840,.T.);
#5096=ORIENTED_EDGE('',*,*,#3843,.F.);
#5097=ORIENTED_EDGE('',*,*,#3842,.T.);
#5098=ORIENTED_EDGE('',*,*,#3844,.F.);
#5099=ORIENTED_EDGE('',*,*,#3845,.T.);
#5100=ORIENTED_EDGE('',*,*,#3846,.F.);
#5101=ORIENTED_EDGE('',*,*,#3845,.F.);
#5102=ORIENTED_EDGE('',*,*,#3847,.F.);
#5103=ORIENTED_EDGE('',*,*,#3848,.T.);
#5104=ORIENTED_EDGE('',*,*,#3849,.F.);
#5105=ORIENTED_EDGE('',*,*,#3848,.F.);
#5106=ORIENTED_EDGE('',*,*,#3850,.F.);
#5107=ORIENTED_EDGE('',*,*,#3851,.T.);
#5108=ORIENTED_EDGE('',*,*,#3852,.F.);
#5109=ORIENTED_EDGE('',*,*,#3851,.F.);
#5110=ORIENTED_EDGE('',*,*,#3853,.F.);
#5111=ORIENTED_EDGE('',*,*,#3854,.T.);
#5112=ORIENTED_EDGE('',*,*,#3855,.F.);
#5113=ORIENTED_EDGE('',*,*,#3854,.F.);
#5114=ORIENTED_EDGE('',*,*,#3856,.F.);
#5115=ORIENTED_EDGE('',*,*,#3857,.F.);
#5116=ORIENTED_EDGE('',*,*,#3858,.F.);
#5117=ORIENTED_EDGE('',*,*,#3859,.F.);
#5118=ORIENTED_EDGE('',*,*,#3860,.T.);
#5119=ORIENTED_EDGE('',*,*,#3853,.T.);
#5120=ORIENTED_EDGE('',*,*,#3850,.T.);
#5121=ORIENTED_EDGE('',*,*,#3847,.T.);
#5122=ORIENTED_EDGE('',*,*,#3844,.T.);
#5123=ORIENTED_EDGE('',*,*,#3857,.T.);
#5124=ORIENTED_EDGE('',*,*,#3861,.T.);
#5125=ORIENTED_EDGE('',*,*,#3862,.F.);
#5126=ORIENTED_EDGE('',*,*,#3863,.F.);
#5127=ORIENTED_EDGE('',*,*,#3858,.T.);
#5128=ORIENTED_EDGE('',*,*,#3863,.T.);
#5129=ORIENTED_EDGE('',*,*,#3864,.F.);
#5130=ORIENTED_EDGE('',*,*,#3865,.F.);
#5131=ORIENTED_EDGE('',*,*,#3859,.T.);
#5132=ORIENTED_EDGE('',*,*,#3865,.T.);
#5133=ORIENTED_EDGE('',*,*,#3866,.F.);
#5134=ORIENTED_EDGE('',*,*,#3867,.F.);
#5135=ORIENTED_EDGE('',*,*,#3856,.T.);
#5136=ORIENTED_EDGE('',*,*,#3867,.T.);
#5137=ORIENTED_EDGE('',*,*,#3868,.F.);
#5138=ORIENTED_EDGE('',*,*,#3861,.F.);
#5139=ORIENTED_EDGE('',*,*,#3868,.T.);
#5140=ORIENTED_EDGE('',*,*,#3866,.T.);
#5141=ORIENTED_EDGE('',*,*,#3864,.T.);
#5142=ORIENTED_EDGE('',*,*,#3862,.T.);
#5143=ORIENTED_EDGE('',*,*,#3846,.T.);
#5144=ORIENTED_EDGE('',*,*,#3849,.T.);
#5145=ORIENTED_EDGE('',*,*,#3852,.T.);
#5146=ORIENTED_EDGE('',*,*,#3855,.T.);
#5147=ORIENTED_EDGE('',*,*,#3860,.F.);
#5148=ORIENTED_EDGE('',*,*,#3869,.T.);
#5149=ORIENTED_EDGE('',*,*,#3870,.F.);
#5150=ORIENTED_EDGE('',*,*,#3869,.F.);
#5151=ORIENTED_EDGE('',*,*,#3871,.F.);
#5152=ORIENTED_EDGE('',*,*,#3872,.T.);
#5153=ORIENTED_EDGE('',*,*,#3873,.F.);
#5154=ORIENTED_EDGE('',*,*,#3872,.F.);
#5155=ORIENTED_EDGE('',*,*,#3874,.F.);
#5156=ORIENTED_EDGE('',*,*,#3875,.T.);
#5157=ORIENTED_EDGE('',*,*,#3876,.F.);
#5158=ORIENTED_EDGE('',*,*,#3877,.F.);
#5159=ORIENTED_EDGE('',*,*,#3874,.T.);
#5160=ORIENTED_EDGE('',*,*,#3878,.F.);
#5161=ORIENTED_EDGE('',*,*,#3879,.F.);
#5162=ORIENTED_EDGE('',*,*,#3880,.F.);
#5163=ORIENTED_EDGE('',*,*,#3877,.T.);
#5164=ORIENTED_EDGE('',*,*,#3881,.T.);
#5165=ORIENTED_EDGE('',*,*,#3882,.T.);
#5166=ORIENTED_EDGE('',*,*,#3878,.T.);
#5167=ORIENTED_EDGE('',*,*,#3870,.T.);
#5168=ORIENTED_EDGE('',*,*,#3873,.T.);
#5169=ORIENTED_EDGE('',*,*,#3876,.T.);
#5170=ORIENTED_EDGE('',*,*,#3883,.F.);
#5171=ORIENTED_EDGE('',*,*,#3884,.F.);
#5172=ORIENTED_EDGE('',*,*,#3881,.F.);
#5173=ORIENTED_EDGE('',*,*,#3884,.T.);
#5174=ORIENTED_EDGE('',*,*,#3885,.T.);
#5175=ORIENTED_EDGE('',*,*,#3879,.T.);
#5176=ORIENTED_EDGE('',*,*,#3882,.F.);
#5177=ORIENTED_EDGE('',*,*,#3880,.T.);
#5178=ORIENTED_EDGE('',*,*,#3885,.F.);
#5179=ORIENTED_EDGE('',*,*,#3883,.T.);
#5180=ORIENTED_EDGE('',*,*,#3875,.F.);
#5181=ORIENTED_EDGE('',*,*,#3871,.T.);
#5182=ORIENTED_EDGE('',*,*,#3886,.T.);
#5183=ORIENTED_EDGE('',*,*,#3887,.F.);
#5184=ORIENTED_EDGE('',*,*,#3888,.F.);
#5185=ORIENTED_EDGE('',*,*,#3886,.F.);
#5186=ORIENTED_EDGE('',*,*,#3889,.T.);
#5187=ORIENTED_EDGE('',*,*,#3887,.T.);
#5188=ORIENTED_EDGE('',*,*,#3889,.F.);
#5189=ORIENTED_EDGE('',*,*,#3888,.T.);
#5190=ORIENTED_EDGE('',*,*,#3890,.T.);
#5191=ORIENTED_EDGE('',*,*,#3891,.T.);
#5192=ORIENTED_EDGE('',*,*,#3890,.F.);
#5193=ORIENTED_EDGE('',*,*,#3891,.F.);
#5194=ORIENTED_EDGE('',*,*,#3892,.F.);
#5195=ORIENTED_EDGE('',*,*,#3893,.T.);
#5196=ORIENTED_EDGE('',*,*,#3894,.T.);
#5197=ORIENTED_EDGE('',*,*,#3893,.F.);
#5198=ORIENTED_EDGE('',*,*,#3895,.F.);
#5199=ORIENTED_EDGE('',*,*,#3896,.T.);
#5200=ORIENTED_EDGE('',*,*,#3897,.T.);
#5201=ORIENTED_EDGE('',*,*,#3896,.F.);
#5202=ORIENTED_EDGE('',*,*,#3895,.T.);
#5203=ORIENTED_EDGE('',*,*,#3892,.T.);
#5204=ORIENTED_EDGE('',*,*,#3897,.F.);
#5205=ORIENTED_EDGE('',*,*,#3894,.F.);
#5206=ORIENTED_EDGE('',*,*,#3898,.F.);
#5207=ORIENTED_EDGE('',*,*,#3899,.T.);
#5208=ORIENTED_EDGE('',*,*,#3900,.F.);
#5209=ORIENTED_EDGE('',*,*,#3901,.F.);
#5210=ORIENTED_EDGE('',*,*,#3902,.F.);
#5211=ORIENTED_EDGE('',*,*,#3903,.T.);
#5212=ORIENTED_EDGE('',*,*,#3904,.F.);
#5213=ORIENTED_EDGE('',*,*,#3905,.F.);
#5214=ORIENTED_EDGE('',*,*,#3903,.F.);
#5215=ORIENTED_EDGE('',*,*,#3906,.F.);
#5216=ORIENTED_EDGE('',*,*,#3899,.F.);
#5217=ORIENTED_EDGE('',*,*,#3907,.F.);
#5218=ORIENTED_EDGE('',*,*,#3901,.T.);
#5219=ORIENTED_EDGE('',*,*,#3908,.F.);
#5220=ORIENTED_EDGE('',*,*,#3909,.T.);
#5221=ORIENTED_EDGE('',*,*,#3910,.T.);
#5222=ORIENTED_EDGE('',*,*,#3909,.F.);
#5223=ORIENTED_EDGE('',*,*,#3906,.T.);
#5224=ORIENTED_EDGE('',*,*,#3902,.T.);
#5225=ORIENTED_EDGE('',*,*,#3907,.T.);
#5226=ORIENTED_EDGE('',*,*,#3900,.T.);
#5227=ORIENTED_EDGE('',*,*,#3898,.T.);
#5228=ORIENTED_EDGE('',*,*,#3911,.F.);
#5229=ORIENTED_EDGE('',*,*,#3912,.T.);
#5230=ORIENTED_EDGE('',*,*,#3913,.T.);
#5231=ORIENTED_EDGE('',*,*,#3912,.F.);
#5232=ORIENTED_EDGE('',*,*,#3904,.T.);
#5233=ORIENTED_EDGE('',*,*,#3905,.T.);
#5234=ORIENTED_EDGE('',*,*,#3911,.T.);
#5235=ORIENTED_EDGE('',*,*,#3908,.T.);
#5236=ORIENTED_EDGE('',*,*,#3913,.F.);
#5237=ORIENTED_EDGE('',*,*,#3910,.F.);
#5238=ORIENTED_EDGE('',*,*,#3914,.F.);
#5239=ORIENTED_EDGE('',*,*,#3915,.T.);
#5240=ORIENTED_EDGE('',*,*,#3916,.F.);
#5241=ORIENTED_EDGE('',*,*,#3915,.F.);
#5242=ORIENTED_EDGE('',*,*,#3914,.T.);
#5243=ORIENTED_EDGE('',*,*,#3917,.F.);
#5244=ORIENTED_EDGE('',*,*,#3918,.T.);
#5245=ORIENTED_EDGE('',*,*,#3919,.T.);
#5246=ORIENTED_EDGE('',*,*,#3918,.F.);
#5247=ORIENTED_EDGE('',*,*,#3919,.F.);
#5248=ORIENTED_EDGE('',*,*,#3920,.T.);
#5249=ORIENTED_EDGE('',*,*,#3921,.F.);
#5250=ORIENTED_EDGE('',*,*,#3922,.F.);
#5251=ORIENTED_EDGE('',*,*,#3923,.F.);
#5252=ORIENTED_EDGE('',*,*,#3920,.F.);
#5253=ORIENTED_EDGE('',*,*,#3924,.T.);
#5254=ORIENTED_EDGE('',*,*,#3922,.T.);
#5255=ORIENTED_EDGE('',*,*,#3924,.F.);
#5256=ORIENTED_EDGE('',*,*,#3923,.T.);
#5257=ORIENTED_EDGE('',*,*,#3925,.T.);
#5258=ORIENTED_EDGE('',*,*,#3926,.T.);
#5259=ORIENTED_EDGE('',*,*,#3925,.F.);
#5260=ORIENTED_EDGE('',*,*,#3927,.F.);
#5261=ORIENTED_EDGE('',*,*,#3928,.T.);
#5262=ORIENTED_EDGE('',*,*,#3921,.T.);
#5263=ORIENTED_EDGE('',*,*,#3928,.F.);
#5264=ORIENTED_EDGE('',*,*,#3927,.T.);
#5265=ORIENTED_EDGE('',*,*,#3916,.T.);
#5266=ORIENTED_EDGE('',*,*,#3926,.F.);
#5267=ORIENTED_EDGE('',*,*,#3917,.T.);
#5268=ORIENTED_EDGE('',*,*,#3929,.F.);
#5269=ORIENTED_EDGE('',*,*,#3930,.T.);
#5270=ORIENTED_EDGE('',*,*,#3931,.T.);
#5271=ORIENTED_EDGE('',*,*,#3930,.F.);
#5272=ORIENTED_EDGE('',*,*,#3932,.F.);
#5273=ORIENTED_EDGE('',*,*,#3933,.T.);
#5274=ORIENTED_EDGE('',*,*,#3934,.T.);
#5275=ORIENTED_EDGE('',*,*,#3933,.F.);
#5276=ORIENTED_EDGE('',*,*,#3932,.T.);
#5277=ORIENTED_EDGE('',*,*,#3929,.T.);
#5278=ORIENTED_EDGE('',*,*,#3934,.F.);
#5279=ORIENTED_EDGE('',*,*,#3931,.F.);
#5280=ORIENTED_EDGE('',*,*,#3935,.F.);
#5281=ORIENTED_EDGE('',*,*,#3936,.T.);
#5282=ORIENTED_EDGE('',*,*,#3937,.T.);
#5283=ORIENTED_EDGE('',*,*,#3936,.F.);
#5284=ORIENTED_EDGE('',*,*,#3938,.F.);
#5285=ORIENTED_EDGE('',*,*,#3939,.T.);
#5286=ORIENTED_EDGE('',*,*,#3940,.T.);
#5287=ORIENTED_EDGE('',*,*,#3939,.F.);
#5288=ORIENTED_EDGE('',*,*,#3938,.T.);
#5289=ORIENTED_EDGE('',*,*,#3935,.T.);
#5290=ORIENTED_EDGE('',*,*,#3940,.F.);
#5291=ORIENTED_EDGE('',*,*,#3937,.F.);
#5292=ORIENTED_EDGE('',*,*,#3941,.F.);
#5293=ORIENTED_EDGE('',*,*,#3942,.T.);
#5294=ORIENTED_EDGE('',*,*,#3943,.T.);
#5295=ORIENTED_EDGE('',*,*,#3942,.F.);
#5296=ORIENTED_EDGE('',*,*,#3944,.F.);
#5297=ORIENTED_EDGE('',*,*,#3945,.T.);
#5298=ORIENTED_EDGE('',*,*,#3946,.T.);
#5299=ORIENTED_EDGE('',*,*,#3945,.F.);
#5300=ORIENTED_EDGE('',*,*,#3944,.T.);
#5301=ORIENTED_EDGE('',*,*,#3941,.T.);
#5302=ORIENTED_EDGE('',*,*,#3946,.F.);
#5303=ORIENTED_EDGE('',*,*,#3943,.F.);
#5304=ORIENTED_EDGE('',*,*,#3947,.F.);
#5305=ORIENTED_EDGE('',*,*,#3948,.T.);
#5306=ORIENTED_EDGE('',*,*,#3949,.T.);
#5307=ORIENTED_EDGE('',*,*,#3948,.F.);
#5308=ORIENTED_EDGE('',*,*,#3950,.F.);
#5309=ORIENTED_EDGE('',*,*,#3951,.T.);
#5310=ORIENTED_EDGE('',*,*,#3952,.T.);
#5311=ORIENTED_EDGE('',*,*,#3951,.F.);
#5312=ORIENTED_EDGE('',*,*,#3950,.T.);
#5313=ORIENTED_EDGE('',*,*,#3947,.T.);
#5314=ORIENTED_EDGE('',*,*,#3952,.F.);
#5315=ORIENTED_EDGE('',*,*,#3949,.F.);
#5316=ORIENTED_EDGE('',*,*,#3953,.F.);
#5317=ORIENTED_EDGE('',*,*,#3954,.F.);
#5318=ORIENTED_EDGE('',*,*,#3955,.T.);
#5319=ORIENTED_EDGE('',*,*,#3956,.T.);
#5320=ORIENTED_EDGE('',*,*,#3957,.F.);
#5321=ORIENTED_EDGE('',*,*,#3958,.F.);
#5322=ORIENTED_EDGE('',*,*,#3959,.T.);
#5323=ORIENTED_EDGE('',*,*,#3960,.T.);
#5324=ORIENTED_EDGE('',*,*,#3955,.F.);
#5325=ORIENTED_EDGE('',*,*,#3961,.F.);
#5326=ORIENTED_EDGE('',*,*,#3962,.T.);
#5327=ORIENTED_EDGE('',*,*,#3963,.T.);
#5328=ORIENTED_EDGE('',*,*,#3959,.F.);
#5329=ORIENTED_EDGE('',*,*,#3964,.F.);
#5330=ORIENTED_EDGE('',*,*,#3965,.T.);
#5331=ORIENTED_EDGE('',*,*,#3966,.T.);
#5332=ORIENTED_EDGE('',*,*,#3962,.F.);
#5333=ORIENTED_EDGE('',*,*,#3967,.F.);
#5334=ORIENTED_EDGE('',*,*,#3968,.T.);
#5335=ORIENTED_EDGE('',*,*,#3969,.T.);
#5336=ORIENTED_EDGE('',*,*,#3965,.F.);
#5337=ORIENTED_EDGE('',*,*,#3970,.F.);
#5338=ORIENTED_EDGE('',*,*,#3957,.T.);
#5339=ORIENTED_EDGE('',*,*,#3971,.T.);
#5340=ORIENTED_EDGE('',*,*,#3968,.F.);
#5341=ORIENTED_EDGE('',*,*,#3971,.F.);
#5342=ORIENTED_EDGE('',*,*,#3956,.F.);
#5343=ORIENTED_EDGE('',*,*,#3960,.F.);
#5344=ORIENTED_EDGE('',*,*,#3963,.F.);
#5345=ORIENTED_EDGE('',*,*,#3966,.F.);
#5346=ORIENTED_EDGE('',*,*,#3969,.F.);
#5347=ORIENTED_EDGE('',*,*,#3972,.F.);
#5348=ORIENTED_EDGE('',*,*,#3954,.T.);
#5349=ORIENTED_EDGE('',*,*,#3970,.T.);
#5350=ORIENTED_EDGE('',*,*,#3967,.T.);
#5351=ORIENTED_EDGE('',*,*,#3964,.T.);
#5352=ORIENTED_EDGE('',*,*,#3961,.T.);
#5353=ORIENTED_EDGE('',*,*,#3958,.T.);
#5354=ORIENTED_EDGE('',*,*,#3973,.F.);
#5355=ORIENTED_EDGE('',*,*,#3974,.T.);
#5356=ORIENTED_EDGE('',*,*,#3972,.T.);
#5357=ORIENTED_EDGE('',*,*,#3974,.F.);
#5358=ORIENTED_EDGE('',*,*,#3953,.T.);
#5359=ORIENTED_EDGE('',*,*,#3975,.T.);
#5360=ORIENTED_EDGE('',*,*,#3973,.T.);
#5361=ORIENTED_EDGE('',*,*,#3975,.F.);
#5362=ORIENTED_EDGE('',*,*,#3976,.F.);
#5363=ORIENTED_EDGE('',*,*,#3977,.F.);
#5364=ORIENTED_EDGE('',*,*,#3978,.T.);
#5365=ORIENTED_EDGE('',*,*,#3976,.T.);
#5366=ORIENTED_EDGE('',*,*,#3978,.F.);
#5367=ORIENTED_EDGE('',*,*,#3979,.F.);
#5368=ORIENTED_EDGE('',*,*,#3980,.T.);
#5369=ORIENTED_EDGE('',*,*,#3977,.T.);
#5370=ORIENTED_EDGE('',*,*,#3980,.F.);
#5371=ORIENTED_EDGE('',*,*,#3981,.F.);
#5372=ORIENTED_EDGE('',*,*,#3982,.T.);
#5373=ORIENTED_EDGE('',*,*,#3979,.T.);
#5374=ORIENTED_EDGE('',*,*,#3982,.F.);
#5375=ORIENTED_EDGE('',*,*,#3981,.T.);
#5376=ORIENTED_EDGE('',*,*,#3983,.F.);
#5377=ORIENTED_EDGE('',*,*,#3984,.F.);
#5378=ORIENTED_EDGE('',*,*,#3985,.T.);
#5379=ORIENTED_EDGE('',*,*,#3983,.T.);
#5380=ORIENTED_EDGE('',*,*,#3985,.F.);
#5381=ORIENTED_EDGE('',*,*,#3986,.F.);
#5382=ORIENTED_EDGE('',*,*,#3987,.T.);
#5383=ORIENTED_EDGE('',*,*,#3984,.T.);
#5384=ORIENTED_EDGE('',*,*,#3987,.F.);
#5385=ORIENTED_EDGE('',*,*,#3988,.F.);
#5386=ORIENTED_EDGE('',*,*,#3989,.T.);
#5387=ORIENTED_EDGE('',*,*,#3986,.T.);
#5388=ORIENTED_EDGE('',*,*,#3989,.F.);
#5389=ORIENTED_EDGE('',*,*,#3988,.T.);
#5390=ORIENTED_EDGE('',*,*,#3990,.T.);
#5391=ORIENTED_EDGE('',*,*,#3991,.T.);
#5392=ORIENTED_EDGE('',*,*,#3992,.T.);
#5393=ORIENTED_EDGE('',*,*,#3993,.F.);
#5394=ORIENTED_EDGE('',*,*,#3994,.T.);
#5395=ORIENTED_EDGE('',*,*,#3995,.T.);
#5396=ORIENTED_EDGE('',*,*,#3996,.T.);
#5397=ORIENTED_EDGE('',*,*,#3991,.F.);
#5398=ORIENTED_EDGE('',*,*,#3997,.T.);
#5399=ORIENTED_EDGE('',*,*,#3998,.T.);
#5400=ORIENTED_EDGE('',*,*,#3999,.T.);
#5401=ORIENTED_EDGE('',*,*,#3995,.F.);
#5402=ORIENTED_EDGE('',*,*,#4000,.T.);
#5403=ORIENTED_EDGE('',*,*,#4001,.T.);
#5404=ORIENTED_EDGE('',*,*,#4002,.T.);
#5405=ORIENTED_EDGE('',*,*,#3998,.F.);
#5406=ORIENTED_EDGE('',*,*,#4003,.T.);
#5407=ORIENTED_EDGE('',*,*,#4004,.T.);
#5408=ORIENTED_EDGE('',*,*,#4005,.T.);
#5409=ORIENTED_EDGE('',*,*,#4001,.F.);
#5410=ORIENTED_EDGE('',*,*,#4006,.T.);
#5411=ORIENTED_EDGE('',*,*,#3993,.T.);
#5412=ORIENTED_EDGE('',*,*,#4007,.T.);
#5413=ORIENTED_EDGE('',*,*,#4004,.F.);
#5414=ORIENTED_EDGE('',*,*,#4006,.F.);
#5415=ORIENTED_EDGE('',*,*,#4003,.F.);
#5416=ORIENTED_EDGE('',*,*,#4000,.F.);
#5417=ORIENTED_EDGE('',*,*,#3997,.F.);
#5418=ORIENTED_EDGE('',*,*,#3994,.F.);
#5419=ORIENTED_EDGE('',*,*,#3990,.F.);
#5420=ORIENTED_EDGE('',*,*,#4007,.F.);
#5421=ORIENTED_EDGE('',*,*,#3992,.F.);
#5422=ORIENTED_EDGE('',*,*,#3996,.F.);
#5423=ORIENTED_EDGE('',*,*,#3999,.F.);
#5424=ORIENTED_EDGE('',*,*,#4002,.F.);
#5425=ORIENTED_EDGE('',*,*,#4005,.F.);
#5426=ORIENTED_EDGE('',*,*,#4008,.T.);
#5427=ORIENTED_EDGE('',*,*,#4009,.T.);
#5428=ORIENTED_EDGE('',*,*,#4010,.T.);
#5429=ORIENTED_EDGE('',*,*,#4011,.F.);
#5430=ORIENTED_EDGE('',*,*,#4012,.T.);
#5431=ORIENTED_EDGE('',*,*,#4013,.T.);
#5432=ORIENTED_EDGE('',*,*,#4014,.T.);
#5433=ORIENTED_EDGE('',*,*,#4009,.F.);
#5434=ORIENTED_EDGE('',*,*,#4015,.T.);
#5435=ORIENTED_EDGE('',*,*,#4016,.T.);
#5436=ORIENTED_EDGE('',*,*,#4017,.T.);
#5437=ORIENTED_EDGE('',*,*,#4013,.F.);
#5438=ORIENTED_EDGE('',*,*,#4018,.T.);
#5439=ORIENTED_EDGE('',*,*,#4019,.T.);
#5440=ORIENTED_EDGE('',*,*,#4020,.T.);
#5441=ORIENTED_EDGE('',*,*,#4016,.F.);
#5442=ORIENTED_EDGE('',*,*,#4021,.T.);
#5443=ORIENTED_EDGE('',*,*,#4022,.T.);
#5444=ORIENTED_EDGE('',*,*,#4023,.T.);
#5445=ORIENTED_EDGE('',*,*,#4019,.F.);
#5446=ORIENTED_EDGE('',*,*,#4024,.T.);
#5447=ORIENTED_EDGE('',*,*,#4011,.T.);
#5448=ORIENTED_EDGE('',*,*,#4025,.T.);
#5449=ORIENTED_EDGE('',*,*,#4022,.F.);
#5450=ORIENTED_EDGE('',*,*,#4024,.F.);
#5451=ORIENTED_EDGE('',*,*,#4021,.F.);
#5452=ORIENTED_EDGE('',*,*,#4018,.F.);
#5453=ORIENTED_EDGE('',*,*,#4015,.F.);
#5454=ORIENTED_EDGE('',*,*,#4012,.F.);
#5455=ORIENTED_EDGE('',*,*,#4008,.F.);
#5456=ORIENTED_EDGE('',*,*,#4025,.F.);
#5457=ORIENTED_EDGE('',*,*,#4010,.F.);
#5458=ORIENTED_EDGE('',*,*,#4014,.F.);
#5459=ORIENTED_EDGE('',*,*,#4017,.F.);
#5460=ORIENTED_EDGE('',*,*,#4020,.F.);
#5461=ORIENTED_EDGE('',*,*,#4023,.F.);
#5462=ORIENTED_EDGE('',*,*,#4026,.F.);
#5463=ORIENTED_EDGE('',*,*,#4027,.F.);
#5464=ORIENTED_EDGE('',*,*,#4028,.F.);
#5465=ORIENTED_EDGE('',*,*,#4029,.T.);
#5466=ORIENTED_EDGE('',*,*,#4027,.T.);
#5467=ORIENTED_EDGE('',*,*,#4029,.F.);
#5468=ORIENTED_EDGE('',*,*,#4030,.F.);
#5469=ORIENTED_EDGE('',*,*,#4031,.T.);
#5470=ORIENTED_EDGE('',*,*,#4028,.T.);
#5471=ORIENTED_EDGE('',*,*,#4031,.F.);
#5472=ORIENTED_EDGE('',*,*,#4032,.F.);
#5473=ORIENTED_EDGE('',*,*,#4033,.T.);
#5474=ORIENTED_EDGE('',*,*,#4030,.T.);
#5475=ORIENTED_EDGE('',*,*,#4033,.F.);
#5476=ORIENTED_EDGE('',*,*,#4032,.T.);
#5477=ORIENTED_EDGE('',*,*,#4034,.F.);
#5478=ORIENTED_EDGE('',*,*,#4035,.F.);
#5479=ORIENTED_EDGE('',*,*,#4036,.T.);
#5480=ORIENTED_EDGE('',*,*,#4034,.T.);
#5481=ORIENTED_EDGE('',*,*,#4036,.F.);
#5482=ORIENTED_EDGE('',*,*,#4026,.T.);
#5483=ORIENTED_EDGE('',*,*,#4037,.T.);
#5484=ORIENTED_EDGE('',*,*,#4035,.T.);
#5485=ORIENTED_EDGE('',*,*,#4037,.F.);
#5486=ORIENTED_EDGE('',*,*,#4038,.F.);
#5487=ORIENTED_EDGE('',*,*,#4039,.T.);
#5488=ORIENTED_EDGE('',*,*,#4040,.F.);
#5489=ORIENTED_EDGE('',*,*,#4039,.F.);
#5490=ORIENTED_EDGE('',*,*,#4041,.F.);
#5491=ORIENTED_EDGE('',*,*,#4042,.T.);
#5492=ORIENTED_EDGE('',*,*,#4043,.F.);
#5493=ORIENTED_EDGE('',*,*,#4042,.F.);
#5494=ORIENTED_EDGE('',*,*,#4044,.F.);
#5495=ORIENTED_EDGE('',*,*,#4045,.F.);
#5496=ORIENTED_EDGE('',*,*,#4046,.F.);
#5497=ORIENTED_EDGE('',*,*,#4047,.T.);
#5498=ORIENTED_EDGE('',*,*,#4044,.T.);
#5499=ORIENTED_EDGE('',*,*,#4048,.F.);
#5500=ORIENTED_EDGE('',*,*,#4049,.F.);
#5501=ORIENTED_EDGE('',*,*,#4050,.F.);
#5502=ORIENTED_EDGE('',*,*,#4047,.F.);
#5503=ORIENTED_EDGE('',*,*,#4051,.T.);
#5504=ORIENTED_EDGE('',*,*,#4052,.F.);
#5505=ORIENTED_EDGE('',*,*,#4048,.T.);
#5506=ORIENTED_EDGE('',*,*,#4038,.T.);
#5507=ORIENTED_EDGE('',*,*,#4041,.T.);
#5508=ORIENTED_EDGE('',*,*,#4046,.T.);
#5509=ORIENTED_EDGE('',*,*,#4053,.F.);
#5510=ORIENTED_EDGE('',*,*,#4054,.F.);
#5511=ORIENTED_EDGE('',*,*,#4051,.F.);
#5512=ORIENTED_EDGE('',*,*,#4049,.T.);
#5513=ORIENTED_EDGE('',*,*,#4052,.T.);
#5514=ORIENTED_EDGE('',*,*,#4054,.T.);
#5515=ORIENTED_EDGE('',*,*,#4055,.F.);
#5516=ORIENTED_EDGE('',*,*,#4050,.T.);
#5517=ORIENTED_EDGE('',*,*,#4055,.T.);
#5518=ORIENTED_EDGE('',*,*,#4053,.T.);
#5519=ORIENTED_EDGE('',*,*,#4045,.T.);
#5520=ORIENTED_EDGE('',*,*,#4040,.T.);
#5521=ORIENTED_EDGE('',*,*,#4043,.T.);
#5522=ORIENTED_EDGE('',*,*,#4056,.F.);
#5523=ORIENTED_EDGE('',*,*,#4057,.T.);
#5524=ORIENTED_EDGE('',*,*,#4058,.T.);
#5525=ORIENTED_EDGE('',*,*,#4057,.F.);
#5526=ORIENTED_EDGE('',*,*,#4059,.F.);
#5527=ORIENTED_EDGE('',*,*,#4060,.T.);
#5528=ORIENTED_EDGE('',*,*,#4061,.T.);
#5529=ORIENTED_EDGE('',*,*,#4060,.F.);
#5530=ORIENTED_EDGE('',*,*,#4059,.T.);
#5531=ORIENTED_EDGE('',*,*,#4056,.T.);
#5532=ORIENTED_EDGE('',*,*,#4061,.F.);
#5533=ORIENTED_EDGE('',*,*,#4058,.F.);
#5534=ORIENTED_EDGE('',*,*,#4062,.F.);
#5535=ORIENTED_EDGE('',*,*,#4063,.T.);
#5536=ORIENTED_EDGE('',*,*,#4064,.T.);
#5537=ORIENTED_EDGE('',*,*,#4063,.F.);
#5538=ORIENTED_EDGE('',*,*,#4065,.F.);
#5539=ORIENTED_EDGE('',*,*,#4066,.T.);
#5540=ORIENTED_EDGE('',*,*,#4067,.T.);
#5541=ORIENTED_EDGE('',*,*,#4066,.F.);
#5542=ORIENTED_EDGE('',*,*,#4065,.T.);
#5543=ORIENTED_EDGE('',*,*,#4062,.T.);
#5544=ORIENTED_EDGE('',*,*,#4067,.F.);
#5545=ORIENTED_EDGE('',*,*,#4064,.F.);
#5546=CYLINDRICAL_SURFACE('',#6562,0.21);
#5547=CYLINDRICAL_SURFACE('',#6565,0.21);
#5548=CYLINDRICAL_SURFACE('',#6568,0.210000000000001);
#5549=CYLINDRICAL_SURFACE('',#6571,0.210000000000001);
#5550=CYLINDRICAL_SURFACE('',#6574,0.21);
#5551=CYLINDRICAL_SURFACE('',#6577,0.21);
#5552=CYLINDRICAL_SURFACE('',#6580,0.21);
#5553=CYLINDRICAL_SURFACE('',#6583,0.21);
#5554=CYLINDRICAL_SURFACE('',#6610,0.525);
#5555=CYLINDRICAL_SURFACE('',#6612,0.525);
#5556=CYLINDRICAL_SURFACE('',#6617,0.525);
#5557=CYLINDRICAL_SURFACE('',#6622,0.525);
#5558=CYLINDRICAL_SURFACE('',#6627,2.2);
#5559=CYLINDRICAL_SURFACE('',#6640,0.165);
#5560=CYLINDRICAL_SURFACE('',#6644,0.165);
#5561=CYLINDRICAL_SURFACE('',#6648,0.165);
#5562=CYLINDRICAL_SURFACE('',#6652,0.165);
#5563=CYLINDRICAL_SURFACE('',#6656,0.25);
#5564=CYLINDRICAL_SURFACE('',#6657,0.275);
#5565=CYLINDRICAL_SURFACE('',#6659,0.275);
#5566=CYLINDRICAL_SURFACE('',#6661,0.275);
#5567=CYLINDRICAL_SURFACE('',#6663,0.275);
#5568=CYLINDRICAL_SURFACE('',#6665,1.5);
#5569=CYLINDRICAL_SURFACE('',#6670,3.);
#5570=CYLINDRICAL_SURFACE('',#6672,1.02);
#5571=CYLINDRICAL_SURFACE('',#6677,1.02);
#5572=CYLINDRICAL_SURFACE('',#6680,1.49);
#5573=CYLINDRICAL_SURFACE('',#6686,0.225);
#5574=CYLINDRICAL_SURFACE('',#6689,0.225);
#5575=CYLINDRICAL_SURFACE('',#6692,0.225);
#5576=CYLINDRICAL_SURFACE('',#6695,0.225);
#5577=CYLINDRICAL_SURFACE('',#6698,1.49);
#5578=CYLINDRICAL_SURFACE('',#6703,1.02);
#5579=CYLINDRICAL_SURFACE('',#6705,2.2);
#5580=CYLINDRICAL_SURFACE('',#6714,0.525);
#5581=CYLINDRICAL_SURFACE('',#6716,0.525);
#5582=CYLINDRICAL_SURFACE('',#6721,0.525);
#5583=CYLINDRICAL_SURFACE('',#6726,0.525);
#5584=CYLINDRICAL_SURFACE('',#6731,2.2);
#5585=CYLINDRICAL_SURFACE('',#6744,0.165);
#5586=CYLINDRICAL_SURFACE('',#6748,0.165);
#5587=CYLINDRICAL_SURFACE('',#6752,0.164999999999999);
#5588=CYLINDRICAL_SURFACE('',#6756,0.164999999999999);
#5589=CYLINDRICAL_SURFACE('',#6760,0.25);
#5590=CYLINDRICAL_SURFACE('',#6761,0.275);
#5591=CYLINDRICAL_SURFACE('',#6763,0.275);
#5592=CYLINDRICAL_SURFACE('',#6765,0.275);
#5593=CYLINDRICAL_SURFACE('',#6767,0.275);
#5594=CYLINDRICAL_SURFACE('',#6769,1.5);
#5595=CYLINDRICAL_SURFACE('',#6774,3.);
#5596=CYLINDRICAL_SURFACE('',#6776,1.02);
#5597=CYLINDRICAL_SURFACE('',#6781,0.225);
#5598=CYLINDRICAL_SURFACE('',#6784,0.225);
#5599=CYLINDRICAL_SURFACE('',#6787,0.225);
#5600=CYLINDRICAL_SURFACE('',#6790,0.225);
#5601=CYLINDRICAL_SURFACE('',#6793,1.49);
#5602=CYLINDRICAL_SURFACE('',#6798,1.02);
#5603=CYLINDRICAL_SURFACE('',#6800,2.2);
#5604=CYLINDRICAL_SURFACE('',#6820,0.425);
#5605=CYLINDRICAL_SURFACE('',#6828,0.24505);
#5606=CYLINDRICAL_SURFACE('',#6837,0.976185);
#5607=CYLINDRICAL_SURFACE('',#6839,0.5);
#5608=CYLINDRICAL_SURFACE('',#6845,0.976185);
#5609=CYLINDRICAL_SURFACE('',#6857,1.023815);
#5610=CYLINDRICAL_SURFACE('',#6864,1.5);
#5611=CYLINDRICAL_SURFACE('',#6869,1.023815);
#5612=CYLINDRICAL_SURFACE('',#6891,1.019052);
#5613=CYLINDRICAL_SURFACE('',#6931,0.980948);
#5614=CYLINDRICAL_SURFACE('',#6945,1.013815);
#5615=CYLINDRICAL_SURFACE('',#6949,0.991185);
#5616=CYLINDRICAL_SURFACE('',#6953,1.013815);
#5617=CYLINDRICAL_SURFACE('',#6957,0.991185);
#5618=CYLINDRICAL_SURFACE('',#6965,0.165);
#5619=CYLINDRICAL_SURFACE('',#6969,0.305);
#5620=CYLINDRICAL_SURFACE('',#6972,0.7);
#5621=CYLINDRICAL_SURFACE('',#6980,1.);
#5622=CYLINDRICAL_SURFACE('',#6987,0.7);
#5623=CYLINDRICAL_SURFACE('',#6988,0.5);
#5624=CYLINDRICAL_SURFACE('',#6990,0.5);
#5625=CYLINDRICAL_SURFACE('',#6995,0.505);
#5626=CYLINDRICAL_SURFACE('',#6998,0.7);
#5627=CYLINDRICAL_SURFACE('',#7004,0.505);
#5628=CYLINDRICAL_SURFACE('',#7007,0.7);
#5629=CYLINDRICAL_SURFACE('',#7015,0.165);
#5630=CYLINDRICAL_SURFACE('',#7018,0.505);
#5631=CYLINDRICAL_SURFACE('',#7021,0.9);
#5632=CYLINDRICAL_SURFACE('',#7029,0.165);
#5633=CYLINDRICAL_SURFACE('',#7032,0.5);
#5634=CYLINDRICAL_SURFACE('',#7035,1.2);
#5635=CYLINDRICAL_SURFACE('',#7041,0.225);
#5636=CYLINDRICAL_SURFACE('',#7044,0.8);
#5637=CYLINDRICAL_SURFACE('',#7050,0.165);
#5638=CYLINDRICAL_SURFACE('',#7054,0.165);
#5639=CYLINDRICAL_SURFACE('',#7064,0.7);
#5640=CYLINDRICAL_SURFACE('',#7065,0.3);
#5641=CYLINDRICAL_SURFACE('',#7067,0.3);
#5642=CYLINDRICAL_SURFACE('',#7072,0.305);
#5643=CYLINDRICAL_SURFACE('',#7075,0.5);
#5644=CYLINDRICAL_SURFACE('',#7081,0.305);
#5645=CYLINDRICAL_SURFACE('',#7084,0.5);
#5646=CYLINDRICAL_SURFACE('',#7090,0.225);
#5647=CYLINDRICAL_SURFACE('',#7093,0.6);
#5648=CYLINDRICAL_SURFACE('',#7099,0.225);
#5649=CYLINDRICAL_SURFACE('',#7102,0.5);
#5650=CYLINDRICAL_SURFACE('',#7119,0.1954);
#5651=CYLINDRICAL_SURFACE('',#7126,0.275);
#5652=CYLINDRICAL_SURFACE('',#7129,0.275);
#5653=CYLINDRICAL_SURFACE('',#7132,0.275);
#5654=CYLINDRICAL_SURFACE('',#7135,0.275);
#5655=CYLINDRICAL_SURFACE('',#7145,0.800000000000001);
#5656=CYLINDRICAL_SURFACE('',#7147,0.305);
#5657=CYLINDRICAL_SURFACE('',#7150,0.699999999999999);
#5658=CYLINDRICAL_SURFACE('',#7157,1.);
#5659=CYLINDRICAL_SURFACE('',#7164,0.699999999999999);
#5660=CYLINDRICAL_SURFACE('',#7165,0.5);
#5661=CYLINDRICAL_SURFACE('',#7169,0.505000000000001);
#5662=CYLINDRICAL_SURFACE('',#7172,0.699999999999999);
#5663=CYLINDRICAL_SURFACE('',#7180,0.165);
#5664=CYLINDRICAL_SURFACE('',#7183,0.505000000000001);
#5665=CYLINDRICAL_SURFACE('',#7186,0.9);
#5666=CYLINDRICAL_SURFACE('',#7192,0.164999999999999);
#5667=CYLINDRICAL_SURFACE('',#7196,0.164999999999999);
#5668=CYLINDRICAL_SURFACE('',#7206,0.699999999999999);
#5669=CYLINDRICAL_SURFACE('',#7207,0.300000000000001);
#5670=CYLINDRICAL_SURFACE('',#7209,0.300000000000001);
#5671=CYLINDRICAL_SURFACE('',#7214,0.305);
#5672=CYLINDRICAL_SURFACE('',#7217,0.5);
#5673=CYLINDRICAL_SURFACE('',#7223,0.305);
#5674=CYLINDRICAL_SURFACE('',#7226,0.5);
#5675=CYLINDRICAL_SURFACE('',#7232,0.225);
#5676=CYLINDRICAL_SURFACE('',#7235,0.6);
#5677=CYLINDRICAL_SURFACE('',#7241,0.225);
#5678=CYLINDRICAL_SURFACE('',#7244,0.5);
#5679=CYLINDRICAL_SURFACE('',#7263,0.1954);
#5680=CYLINDRICAL_SURFACE('',#7269,0.35);
#5681=CYLINDRICAL_SURFACE('',#7277,0.1954);
#5682=CYLINDRICAL_SURFACE('',#7305,0.35);
#5683=CYLINDRICAL_SURFACE('',#7313,0.1954);
#5684=CYLINDRICAL_SURFACE('',#7370,0.5);
#5685=CYLINDRICAL_SURFACE('',#7373,0.5);
#5686=CYLINDRICAL_SURFACE('',#7376,1.);
#5687=CYLINDRICAL_SURFACE('',#7383,1.);
#5688=CYLINDRICAL_SURFACE('',#7387,0.305);
#5689=CYLINDRICAL_SURFACE('',#7390,0.5);
#5690=CYLINDRICAL_SURFACE('',#7396,0.305);
#5691=CYLINDRICAL_SURFACE('',#7399,0.5);
#5692=ADVANCED_FACE('',(#886),#5546,.F.);
#5693=ADVANCED_FACE('',(#887),#5547,.F.);
#5694=ADVANCED_FACE('',(#888),#5548,.F.);
#5695=ADVANCED_FACE('',(#889),#5549,.F.);
#5696=ADVANCED_FACE('',(#890),#5550,.F.);
#5697=ADVANCED_FACE('',(#891),#5551,.F.);
#5698=ADVANCED_FACE('',(#892),#5552,.F.);
#5699=ADVANCED_FACE('',(#893),#5553,.F.);
#5700=ADVANCED_FACE('',(#894),#692,.T.);
#5701=ADVANCED_FACE('',(#895),#693,.T.);
#5702=ADVANCED_FACE('',(#896),#694,.T.);
#5703=ADVANCED_FACE('',(#897),#695,.T.);
#5704=ADVANCED_FACE('',(#898,#530,#531,#532,#533,#534,#535,#536,#537),#696,
 .T.);
#5705=ADVANCED_FACE('',(#899,#538,#539,#540,#541,#542,#543,#544,#545),#697,
 .F.);
#5706=ADVANCED_FACE('',(#900),#698,.T.);
#5707=ADVANCED_FACE('',(#901),#699,.T.);
#5708=ADVANCED_FACE('',(#902),#700,.T.);
#5709=ADVANCED_FACE('',(#903),#701,.T.);
#5710=ADVANCED_FACE('',(#904),#702,.T.);
#5711=ADVANCED_FACE('',(#905),#703,.F.);
#5712=ADVANCED_FACE('',(#906),#704,.T.);
#5713=ADVANCED_FACE('',(#907),#705,.T.);
#5714=ADVANCED_FACE('',(#908),#706,.T.);
#5715=ADVANCED_FACE('',(#909),#707,.T.);
#5716=ADVANCED_FACE('',(#910),#708,.T.);
#5717=ADVANCED_FACE('',(#911),#709,.F.);
#5718=ADVANCED_FACE('',(#912),#710,.F.);
#5719=ADVANCED_FACE('',(#913),#5554,.F.);
#5720=ADVANCED_FACE('',(#914),#5555,.F.);
#5721=ADVANCED_FACE('',(#915),#711,.F.);
#5722=ADVANCED_FACE('',(#916),#5556,.F.);
#5723=ADVANCED_FACE('',(#917),#712,.F.);
#5724=ADVANCED_FACE('',(#918),#5557,.F.);
#5725=ADVANCED_FACE('',(#919),#713,.F.);
#5726=ADVANCED_FACE('',(#920),#5558,.T.);
#5727=ADVANCED_FACE('',(#921,#546,#547,#548,#549,#550),#714,.T.);
#5728=ADVANCED_FACE('',(#922),#5559,.F.);
#5729=ADVANCED_FACE('',(#923),#715,.T.);
#5730=ADVANCED_FACE('',(#924),#5560,.F.);
#5731=ADVANCED_FACE('',(#925),#716,.T.);
#5732=ADVANCED_FACE('',(#926),#5561,.F.);
#5733=ADVANCED_FACE('',(#927),#717,.T.);
#5734=ADVANCED_FACE('',(#928),#5562,.F.);
#5735=ADVANCED_FACE('',(#929),#718,.T.);
#5736=ADVANCED_FACE('',(#930),#5563,.F.);
#5737=ADVANCED_FACE('',(#931),#5564,.F.);
#5738=ADVANCED_FACE('',(#932),#5565,.F.);
#5739=ADVANCED_FACE('',(#933),#5566,.F.);
#5740=ADVANCED_FACE('',(#934),#5567,.F.);
#5741=ADVANCED_FACE('',(#935),#5568,.F.);
#5742=ADVANCED_FACE('',(#936,#551),#719,.T.);
#5743=ADVANCED_FACE('',(#937,#552),#5569,.T.);
#5744=ADVANCED_FACE('',(#938,#553),#5570,.F.);
#5745=ADVANCED_FACE('',(#939,#554,#555,#556,#557,#558),#720,.T.);
#5746=ADVANCED_FACE('',(#940,#559,#560,#561,#562,#563),#721,.F.);
#5747=ADVANCED_FACE('',(#941),#5571,.F.);
#5748=ADVANCED_FACE('',(#942),#5572,.T.);
#5749=ADVANCED_FACE('',(#943,#564),#722,.T.);
#5750=ADVANCED_FACE('',(#944,#565),#723,.F.);
#5751=ADVANCED_FACE('',(#945),#5573,.F.);
#5752=ADVANCED_FACE('',(#946),#5574,.F.);
#5753=ADVANCED_FACE('',(#947),#5575,.F.);
#5754=ADVANCED_FACE('',(#948),#5576,.F.);
#5755=ADVANCED_FACE('',(#949),#5577,.T.);
#5756=ADVANCED_FACE('',(#950,#566),#724,.F.);
#5757=ADVANCED_FACE('',(#951),#5578,.F.);
#5758=ADVANCED_FACE('',(#952),#5579,.T.);
#5759=ADVANCED_FACE('',(#953,#567,#568,#569,#570,#571),#725,.T.);
#5760=ADVANCED_FACE('',(#954,#572,#573,#574,#575,#576),#726,.F.);
#5761=ADVANCED_FACE('',(#955),#727,.F.);
#5762=ADVANCED_FACE('',(#956),#5580,.F.);
#5763=ADVANCED_FACE('',(#957),#5581,.F.);
#5764=ADVANCED_FACE('',(#958),#728,.F.);
#5765=ADVANCED_FACE('',(#959),#5582,.F.);
#5766=ADVANCED_FACE('',(#960),#729,.F.);
#5767=ADVANCED_FACE('',(#961),#5583,.F.);
#5768=ADVANCED_FACE('',(#962),#730,.F.);
#5769=ADVANCED_FACE('',(#963),#5584,.T.);
#5770=ADVANCED_FACE('',(#964,#577,#578,#579,#580,#581),#731,.T.);
#5771=ADVANCED_FACE('',(#965),#5585,.F.);
#5772=ADVANCED_FACE('',(#966),#732,.T.);
#5773=ADVANCED_FACE('',(#967),#5586,.F.);
#5774=ADVANCED_FACE('',(#968),#733,.T.);
#5775=ADVANCED_FACE('',(#969),#5587,.F.);
#5776=ADVANCED_FACE('',(#970),#734,.T.);
#5777=ADVANCED_FACE('',(#971),#5588,.F.);
#5778=ADVANCED_FACE('',(#972),#735,.T.);
#5779=ADVANCED_FACE('',(#973),#5589,.F.);
#5780=ADVANCED_FACE('',(#974),#5590,.F.);
#5781=ADVANCED_FACE('',(#975),#5591,.F.);
#5782=ADVANCED_FACE('',(#976),#5592,.F.);
#5783=ADVANCED_FACE('',(#977),#5593,.F.);
#5784=ADVANCED_FACE('',(#978),#5594,.F.);
#5785=ADVANCED_FACE('',(#979,#582),#736,.T.);
#5786=ADVANCED_FACE('',(#980,#583),#5595,.T.);
#5787=ADVANCED_FACE('',(#981,#584),#5596,.F.);
#5788=ADVANCED_FACE('',(#982,#585,#586,#587,#588,#589),#737,.T.);
#5789=ADVANCED_FACE('',(#983,#590,#591,#592,#593,#594),#738,.F.);
#5790=ADVANCED_FACE('',(#984),#5597,.F.);
#5791=ADVANCED_FACE('',(#985),#5598,.F.);
#5792=ADVANCED_FACE('',(#986),#5599,.F.);
#5793=ADVANCED_FACE('',(#987),#5600,.F.);
#5794=ADVANCED_FACE('',(#988),#5601,.T.);
#5795=ADVANCED_FACE('',(#989,#595),#739,.F.);
#5796=ADVANCED_FACE('',(#990),#5602,.F.);
#5797=ADVANCED_FACE('',(#991),#5603,.T.);
#5798=ADVANCED_FACE('',(#992,#596,#597,#598,#599,#600),#740,.T.);
#5799=ADVANCED_FACE('',(#993,#601,#602,#603,#604,#605),#741,.F.);
#5800=ADVANCED_FACE('',(#994),#742,.F.);
#5801=ADVANCED_FACE('',(#995),#743,.F.);
#5802=ADVANCED_FACE('',(#996),#744,.F.);
#5803=ADVANCED_FACE('',(#997),#745,.F.);
#5804=ADVANCED_FACE('',(#998),#746,.F.);
#5805=ADVANCED_FACE('',(#999),#747,.F.);
#5806=ADVANCED_FACE('',(#1000),#748,.F.);
#5807=ADVANCED_FACE('',(#1001),#749,.F.);
#5808=ADVANCED_FACE('',(#1002),#750,.F.);
#5809=ADVANCED_FACE('',(#1003),#751,.T.);
#5810=ADVANCED_FACE('',(#1004),#293,.T.);
#5811=ADVANCED_FACE('',(#1005),#5604,.T.);
#5812=ADVANCED_FACE('',(#1006),#294,.T.);
#5813=ADVANCED_FACE('',(#1007,#606),#752,.T.);
#5814=ADVANCED_FACE('',(#1008),#295,.T.);
#5815=ADVANCED_FACE('',(#1009),#5605,.T.);
#5816=ADVANCED_FACE('',(#1010),#291,.F.);
#5817=ADVANCED_FACE('',(#1011),#5606,.T.);
#5818=ADVANCED_FACE('',(#1012),#5607,.F.);
#5819=ADVANCED_FACE('',(#1013),#296,.F.);
#5820=ADVANCED_FACE('',(#1014,#607),#753,.T.);
#5821=ADVANCED_FACE('',(#1015),#5608,.T.);
#5822=ADVANCED_FACE('',(#1016,#608),#754,.T.);
#5823=ADVANCED_FACE('',(#1017),#297,.F.);
#5824=ADVANCED_FACE('',(#1018),#292,.F.);
#5825=ADVANCED_FACE('',(#1019),#5609,.F.);
#5826=ADVANCED_FACE('',(#1020,#609),#755,.T.);
#5827=ADVANCED_FACE('',(#1021),#298,.T.);
#5828=ADVANCED_FACE('',(#1022),#5610,.T.);
#5829=ADVANCED_FACE('',(#1023),#299,.T.);
#5830=ADVANCED_FACE('',(#1024,#610),#756,.T.);
#5831=ADVANCED_FACE('',(#1025),#5611,.F.);
#5832=ADVANCED_FACE('',(#1026),#275,.T.);
#5833=ADVANCED_FACE('',(#1027),#276,.T.);
#5834=ADVANCED_FACE('',(#1028),#277,.T.);
#5835=ADVANCED_FACE('',(#1029),#278,.T.);
#5836=ADVANCED_FACE('',(#1030),#279,.T.);
#5837=ADVANCED_FACE('',(#1031),#280,.T.);
#5838=ADVANCED_FACE('',(#1032),#281,.T.);
#5839=ADVANCED_FACE('',(#1033),#282,.T.);
#5840=ADVANCED_FACE('',(#1034),#283,.F.);
#5841=ADVANCED_FACE('',(#1035),#5612,.T.);
#5842=ADVANCED_FACE('',(#1036),#757,.T.);
#5843=ADVANCED_FACE('',(#1037),#284,.F.);
#5844=ADVANCED_FACE('',(#1038),#758,.T.);
#5845=ADVANCED_FACE('',(#1039),#285,.F.);
#5846=ADVANCED_FACE('',(#1040),#759,.T.);
#5847=ADVANCED_FACE('',(#1041),#286,.F.);
#5848=ADVANCED_FACE('',(#1042),#760,.T.);
#5849=ADVANCED_FACE('',(#1043),#287,.F.);
#5850=ADVANCED_FACE('',(#1044),#761,.T.);
#5851=ADVANCED_FACE('',(#1045),#288,.F.);
#5852=ADVANCED_FACE('',(#1046),#762,.T.);
#5853=ADVANCED_FACE('',(#1047),#289,.F.);
#5854=ADVANCED_FACE('',(#1048),#5613,.F.);
#5855=ADVANCED_FACE('',(#1049),#763,.T.);
#5856=ADVANCED_FACE('',(#1050),#290,.F.);
#5857=ADVANCED_FACE('',(#1051,#611),#764,.T.);
#5858=ADVANCED_FACE('',(#1052),#765,.T.);
#5859=ADVANCED_FACE('',(#1053,#612),#766,.T.);
#5860=ADVANCED_FACE('',(#1054),#5614,.T.);
#5861=ADVANCED_FACE('',(#1055,#613),#767,.T.);
#5862=ADVANCED_FACE('',(#1056),#5615,.F.);
#5863=ADVANCED_FACE('',(#1057,#614),#768,.T.);
#5864=ADVANCED_FACE('',(#1058),#5616,.T.);
#5865=ADVANCED_FACE('',(#1059,#615),#769,.T.);
#5866=ADVANCED_FACE('',(#1060),#5617,.F.);
#5867=ADVANCED_FACE('',(#1061),#5618,.F.);
#5868=ADVANCED_FACE('',(#1062),#770,.T.);
#5869=ADVANCED_FACE('',(#1063),#5619,.F.);
#5870=ADVANCED_FACE('',(#1064),#5620,.T.);
#5871=ADVANCED_FACE('',(#1065),#771,.T.);
#5872=ADVANCED_FACE('',(#1066,#616,#617),#772,.T.);
#5873=ADVANCED_FACE('',(#1067),#773,.T.);
#5874=ADVANCED_FACE('',(#1068),#5621,.T.);
#5875=ADVANCED_FACE('',(#1069,#618,#619),#774,.F.);
#5876=ADVANCED_FACE('',(#1070,#620),#775,.F.);
#5877=ADVANCED_FACE('',(#1071),#5622,.T.);
#5878=ADVANCED_FACE('',(#1072),#5623,.T.);
#5879=ADVANCED_FACE('',(#1073),#5624,.T.);
#5880=ADVANCED_FACE('',(#1074,#621),#776,.T.);
#5881=ADVANCED_FACE('',(#1075),#777,.F.);
#5882=ADVANCED_FACE('',(#1076),#5625,.F.);
#5883=ADVANCED_FACE('',(#1077),#5626,.T.);
#5884=ADVANCED_FACE('',(#1078,#622),#778,.T.);
#5885=ADVANCED_FACE('',(#1079,#623),#779,.F.);
#5886=ADVANCED_FACE('',(#1080),#5627,.F.);
#5887=ADVANCED_FACE('',(#1081),#5628,.T.);
#5888=ADVANCED_FACE('',(#1082,#624),#780,.T.);
#5889=ADVANCED_FACE('',(#1083,#625),#781,.F.);
#5890=ADVANCED_FACE('',(#1084),#782,.T.);
#5891=ADVANCED_FACE('',(#1085),#5629,.F.);
#5892=ADVANCED_FACE('',(#1086),#783,.T.);
#5893=ADVANCED_FACE('',(#1087,#626),#5630,.F.);
#5894=ADVANCED_FACE('',(#1088,#627),#5631,.T.);
#5895=ADVANCED_FACE('',(#1089,#628),#784,.T.);
#5896=ADVANCED_FACE('',(#1090,#629),#785,.F.);
#5897=ADVANCED_FACE('',(#1091),#786,.T.);
#5898=ADVANCED_FACE('',(#1092),#5632,.F.);
#5899=ADVANCED_FACE('',(#1093),#787,.T.);
#5900=ADVANCED_FACE('',(#1094,#630),#5633,.F.);
#5901=ADVANCED_FACE('',(#1095,#631),#5634,.T.);
#5902=ADVANCED_FACE('',(#1096,#632),#788,.T.);
#5903=ADVANCED_FACE('',(#1097,#633),#789,.F.);
#5904=ADVANCED_FACE('',(#1098),#5635,.F.);
#5905=ADVANCED_FACE('',(#1099),#5636,.T.);
#5906=ADVANCED_FACE('',(#1100,#634),#790,.T.);
#5907=ADVANCED_FACE('',(#1101,#635),#791,.F.);
#5908=ADVANCED_FACE('',(#1102),#5637,.F.);
#5909=ADVANCED_FACE('',(#1103),#792,.T.);
#5910=ADVANCED_FACE('',(#1104),#5638,.F.);
#5911=ADVANCED_FACE('',(#1105),#793,.F.);
#5912=ADVANCED_FACE('',(#1106,#636),#794,.T.);
#5913=ADVANCED_FACE('',(#1107,#637),#795,.F.);
#5914=ADVANCED_FACE('',(#1108),#5639,.T.);
#5915=ADVANCED_FACE('',(#1109),#5640,.T.);
#5916=ADVANCED_FACE('',(#1110),#5641,.T.);
#5917=ADVANCED_FACE('',(#1111,#638),#796,.T.);
#5918=ADVANCED_FACE('',(#1112,#639),#797,.F.);
#5919=ADVANCED_FACE('',(#1113),#5642,.F.);
#5920=ADVANCED_FACE('',(#1114),#5643,.T.);
#5921=ADVANCED_FACE('',(#1115,#640),#798,.T.);
#5922=ADVANCED_FACE('',(#1116,#641),#799,.F.);
#5923=ADVANCED_FACE('',(#1117),#5644,.F.);
#5924=ADVANCED_FACE('',(#1118),#5645,.T.);
#5925=ADVANCED_FACE('',(#1119,#642),#800,.T.);
#5926=ADVANCED_FACE('',(#1120,#643),#801,.F.);
#5927=ADVANCED_FACE('',(#1121),#5646,.F.);
#5928=ADVANCED_FACE('',(#1122),#5647,.T.);
#5929=ADVANCED_FACE('',(#1123,#644),#802,.T.);
#5930=ADVANCED_FACE('',(#1124,#645),#803,.F.);
#5931=ADVANCED_FACE('',(#1125),#5648,.F.);
#5932=ADVANCED_FACE('',(#1126),#5649,.T.);
#5933=ADVANCED_FACE('',(#1127,#646),#804,.T.);
#5934=ADVANCED_FACE('',(#1128,#647),#805,.F.);
#5935=ADVANCED_FACE('',(#1129),#806,.F.);
#5936=ADVANCED_FACE('',(#1130),#807,.F.);
#5937=ADVANCED_FACE('',(#1131),#808,.F.);
#5938=ADVANCED_FACE('',(#1132),#809,.F.);
#5939=ADVANCED_FACE('',(#1133),#810,.F.);
#5940=ADVANCED_FACE('',(#1134),#811,.F.);
#5941=ADVANCED_FACE('',(#1135),#812,.F.);
#5942=ADVANCED_FACE('',(#1136,#648),#813,.T.);
#5943=ADVANCED_FACE('',(#1137),#300,.T.);
#5944=ADVANCED_FACE('',(#1138),#5650,.T.);
#5945=ADVANCED_FACE('',(#1139),#301,.T.);
#5946=ADVANCED_FACE('',(#1140),#814,.T.);
#5947=ADVANCED_FACE('',(#1141),#5651,.F.);
#5948=ADVANCED_FACE('',(#1142),#5652,.F.);
#5949=ADVANCED_FACE('',(#1143),#5653,.F.);
#5950=ADVANCED_FACE('',(#1144),#5654,.F.);
#5951=ADVANCED_FACE('',(#1145,#649,#650,#651,#652,#653),#815,.F.);
#5952=ADVANCED_FACE('',(#1146),#816,.T.);
#5953=ADVANCED_FACE('',(#1147),#817,.T.);
#5954=ADVANCED_FACE('',(#1148),#818,.T.);
#5955=ADVANCED_FACE('',(#1149),#819,.T.);
#5956=ADVANCED_FACE('',(#1150,#654,#655,#656,#657),#820,.T.);
#5957=ADVANCED_FACE('',(#1151),#5655,.T.);
#5958=ADVANCED_FACE('',(#1152),#5656,.F.);
#5959=ADVANCED_FACE('',(#1153),#5657,.T.);
#5960=ADVANCED_FACE('',(#1154),#821,.T.);
#5961=ADVANCED_FACE('',(#1155,#658,#659),#822,.T.);
#5962=ADVANCED_FACE('',(#1156),#823,.T.);
#5963=ADVANCED_FACE('',(#1157),#5658,.T.);
#5964=ADVANCED_FACE('',(#1158,#660,#661),#824,.F.);
#5965=ADVANCED_FACE('',(#1159,#662),#825,.F.);
#5966=ADVANCED_FACE('',(#1160),#5659,.T.);
#5967=ADVANCED_FACE('',(#1161),#5660,.T.);
#5968=ADVANCED_FACE('',(#1162),#826,.F.);
#5969=ADVANCED_FACE('',(#1163),#5661,.F.);
#5970=ADVANCED_FACE('',(#1164),#5662,.T.);
#5971=ADVANCED_FACE('',(#1165,#663),#827,.T.);
#5972=ADVANCED_FACE('',(#1166,#664),#828,.F.);
#5973=ADVANCED_FACE('',(#1167),#829,.T.);
#5974=ADVANCED_FACE('',(#1168),#5663,.F.);
#5975=ADVANCED_FACE('',(#1169),#830,.T.);
#5976=ADVANCED_FACE('',(#1170,#665),#5664,.F.);
#5977=ADVANCED_FACE('',(#1171,#666),#5665,.T.);
#5978=ADVANCED_FACE('',(#1172,#667),#831,.T.);
#5979=ADVANCED_FACE('',(#1173,#668),#832,.F.);
#5980=ADVANCED_FACE('',(#1174),#5666,.F.);
#5981=ADVANCED_FACE('',(#1175),#833,.T.);
#5982=ADVANCED_FACE('',(#1176),#5667,.F.);
#5983=ADVANCED_FACE('',(#1177),#834,.F.);
#5984=ADVANCED_FACE('',(#1178,#669),#835,.T.);
#5985=ADVANCED_FACE('',(#1179,#670),#836,.F.);
#5986=ADVANCED_FACE('',(#1180),#5668,.T.);
#5987=ADVANCED_FACE('',(#1181),#5669,.T.);
#5988=ADVANCED_FACE('',(#1182),#5670,.T.);
#5989=ADVANCED_FACE('',(#1183,#671),#837,.T.);
#5990=ADVANCED_FACE('',(#1184,#672),#838,.F.);
#5991=ADVANCED_FACE('',(#1185),#5671,.F.);
#5992=ADVANCED_FACE('',(#1186),#5672,.T.);
#5993=ADVANCED_FACE('',(#1187,#673),#839,.T.);
#5994=ADVANCED_FACE('',(#1188,#674),#840,.F.);
#5995=ADVANCED_FACE('',(#1189),#5673,.F.);
#5996=ADVANCED_FACE('',(#1190),#5674,.T.);
#5997=ADVANCED_FACE('',(#1191,#675),#841,.T.);
#5998=ADVANCED_FACE('',(#1192,#676),#842,.F.);
#5999=ADVANCED_FACE('',(#1193),#5675,.F.);
#6000=ADVANCED_FACE('',(#1194),#5676,.T.);
#6001=ADVANCED_FACE('',(#1195,#677),#843,.T.);
#6002=ADVANCED_FACE('',(#1196,#678),#844,.F.);
#6003=ADVANCED_FACE('',(#1197),#5677,.F.);
#6004=ADVANCED_FACE('',(#1198),#5678,.T.);
#6005=ADVANCED_FACE('',(#1199,#679),#845,.T.);
#6006=ADVANCED_FACE('',(#1200,#680),#846,.F.);
#6007=ADVANCED_FACE('',(#1201),#847,.F.);
#6008=ADVANCED_FACE('',(#1202),#848,.F.);
#6009=ADVANCED_FACE('',(#1203),#849,.F.);
#6010=ADVANCED_FACE('',(#1204),#850,.F.);
#6011=ADVANCED_FACE('',(#1205),#851,.F.);
#6012=ADVANCED_FACE('',(#1206),#852,.F.);
#6013=ADVANCED_FACE('',(#1207),#853,.F.);
#6014=ADVANCED_FACE('',(#1208),#854,.F.);
#6015=ADVANCED_FACE('',(#1209,#681),#855,.T.);
#6016=ADVANCED_FACE('',(#1210),#302,.T.);
#6017=ADVANCED_FACE('',(#1211),#5679,.T.);
#6018=ADVANCED_FACE('',(#1212),#856,.T.);
#6019=ADVANCED_FACE('',(#1213),#303,.T.);
#6020=ADVANCED_FACE('',(#1214),#5680,.T.);
#6021=ADVANCED_FACE('',(#1215),#304,.T.);
#6022=ADVANCED_FACE('',(#1216,#682),#857,.T.);
#6023=ADVANCED_FACE('',(#1217),#305,.T.);
#6024=ADVANCED_FACE('',(#1218),#5681,.T.);
#6025=ADVANCED_FACE('',(#1219),#306,.T.);
#6026=ADVANCED_FACE('',(#1220),#858,.T.);
#6027=ADVANCED_FACE('',(#1221),#859,.F.);
#6028=ADVANCED_FACE('',(#1222),#860,.F.);
#6029=ADVANCED_FACE('',(#1223),#861,.F.);
#6030=ADVANCED_FACE('',(#1224),#862,.F.);
#6031=ADVANCED_FACE('',(#1225),#863,.F.);
#6032=ADVANCED_FACE('',(#1226),#864,.F.);
#6033=ADVANCED_FACE('',(#1227),#865,.F.);
#6034=ADVANCED_FACE('',(#1228),#866,.F.);
#6035=ADVANCED_FACE('',(#1229),#867,.F.);
#6036=ADVANCED_FACE('',(#1230),#868,.F.);
#6037=ADVANCED_FACE('',(#1231),#869,.F.);
#6038=ADVANCED_FACE('',(#1232),#870,.F.);
#6039=ADVANCED_FACE('',(#1233),#871,.F.);
#6040=ADVANCED_FACE('',(#1234),#872,.F.);
#6041=ADVANCED_FACE('',(#1235),#873,.F.);
#6042=ADVANCED_FACE('',(#1236),#874,.F.);
#6043=ADVANCED_FACE('',(#1237),#875,.F.);
#6044=ADVANCED_FACE('',(#1238),#876,.T.);
#6045=ADVANCED_FACE('',(#1239),#307,.T.);
#6046=ADVANCED_FACE('',(#1240),#5682,.T.);
#6047=ADVANCED_FACE('',(#1241),#308,.T.);
#6048=ADVANCED_FACE('',(#1242,#683),#877,.T.);
#6049=ADVANCED_FACE('',(#1243),#309,.T.);
#6050=ADVANCED_FACE('',(#1244),#5683,.T.);
#6051=ADVANCED_FACE('',(#1245),#5684,.F.);
#6052=ADVANCED_FACE('',(#1246),#5685,.F.);
#6053=ADVANCED_FACE('',(#1247),#5686,.T.);
#6054=ADVANCED_FACE('',(#1248),#878,.T.);
#6055=ADVANCED_FACE('',(#1249,#684,#685),#879,.F.);
#6056=ADVANCED_FACE('',(#1250),#880,.T.);
#6057=ADVANCED_FACE('',(#1251),#5687,.T.);
#6058=ADVANCED_FACE('',(#1252,#686,#687),#881,.T.);
#6059=ADVANCED_FACE('',(#1253),#5688,.F.);
#6060=ADVANCED_FACE('',(#1254),#5689,.T.);
#6061=ADVANCED_FACE('',(#1255,#688),#882,.T.);
#6062=ADVANCED_FACE('',(#1256,#689),#883,.F.);
#6063=ADVANCED_FACE('',(#1257),#5690,.F.);
#6064=ADVANCED_FACE('',(#1258),#5691,.T.);
#6065=ADVANCED_FACE('',(#1259,#690),#884,.T.);
#6066=ADVANCED_FACE('',(#1260,#691),#885,.F.);
#6067=CLOSED_SHELL('',(#5692,#5693,#5694,#5695,#5696,#5697,#5698,#5699,
#5700,#5701,#5702,#5703,#5704,#5705));
#6068=CLOSED_SHELL('',(#5706,#5707,#5708,#5709,#5710,#5711));
#6069=CLOSED_SHELL('',(#5712,#5713,#5714,#5715,#5716,#5717));
#6070=CLOSED_SHELL('',(#5718,#5719,#5720,#5721,#5722,#5723,#5724,#5725,
#5726,#5727,#5728,#5729,#5730,#5731,#5732,#5733,#5734,#5735,#5736,#5737,
#5738,#5739,#5740,#5741,#5742,#5743,#5744,#5745,#5746));
#6071=CLOSED_SHELL('',(#5747,#5748,#5749,#5750));
#6072=CLOSED_SHELL('',(#5751,#5752,#5753,#5754,#5755,#5756,#5757,#5758,
#5759,#5760));
#6073=CLOSED_SHELL('',(#5761,#5762,#5763,#5764,#5765,#5766,#5767,#5768,
#5769,#5770,#5771,#5772,#5773,#5774,#5775,#5776,#5777,#5778,#5779,#5780,
#5781,#5782,#5783,#5784,#5785,#5786,#5787,#5788,#5789));
#6074=CLOSED_SHELL('',(#5790,#5791,#5792,#5793,#5794,#5795,#5796,#5797,
#5798,#5799));
#6075=CLOSED_SHELL('',(#5800,#5801,#5802,#5803,#5804,#5805,#5806,#5807));
#6076=CLOSED_SHELL('',(#5808,#5809,#5810,#5811,#5812,#5813,#5814,#5815));
#6077=CLOSED_SHELL('',(#5816,#5817,#5818,#5819,#5820,#5821,#5822,#5823));
#6078=CLOSED_SHELL('',(#5824,#5825,#5826,#5827,#5828,#5829,#5830,#5831));
#6079=CLOSED_SHELL('',(#5832));
#6080=CLOSED_SHELL('',(#5833));
#6081=CLOSED_SHELL('',(#5834));
#6082=CLOSED_SHELL('',(#5835));
#6083=CLOSED_SHELL('',(#5836));
#6084=CLOSED_SHELL('',(#5837));
#6085=CLOSED_SHELL('',(#5838));
#6086=CLOSED_SHELL('',(#5839));
#6087=CLOSED_SHELL('',(#5840,#5841,#5842,#5843,#5844,#5845,#5846,#5847,
#5848,#5849,#5850,#5851,#5852,#5853,#5854,#5855,#5856,#5857,#5858));
#6088=CLOSED_SHELL('',(#5859,#5860,#5861,#5862));
#6089=CLOSED_SHELL('',(#5863,#5864,#5865,#5866));
#6090=CLOSED_SHELL('',(#5867,#5868,#5869,#5870,#5871,#5872,#5873,#5874,
#5875,#5876,#5877,#5878,#5879,#5880,#5881));
#6091=CLOSED_SHELL('',(#5882,#5883,#5884,#5885));
#6092=CLOSED_SHELL('',(#5886,#5887,#5888,#5889));
#6093=CLOSED_SHELL('',(#5890,#5891,#5892,#5893,#5894,#5895,#5896));
#6094=CLOSED_SHELL('',(#5897,#5898,#5899,#5900,#5901,#5902,#5903));
#6095=CLOSED_SHELL('',(#5904,#5905,#5906,#5907));
#6096=CLOSED_SHELL('',(#5908,#5909,#5910,#5911,#5912,#5913,#5914,#5915,
#5916,#5917,#5918));
#6097=CLOSED_SHELL('',(#5919,#5920,#5921,#5922));
#6098=CLOSED_SHELL('',(#5923,#5924,#5925,#5926));
#6099=CLOSED_SHELL('',(#5927,#5928,#5929,#5930));
#6100=CLOSED_SHELL('',(#5931,#5932,#5933,#5934));
#6101=CLOSED_SHELL('',(#5935,#5936,#5937,#5938,#5939,#5940,#5941,#5942,
#5943,#5944,#5945,#5946));
#6102=CLOSED_SHELL('',(#5947,#5948,#5949,#5950,#5951,#5952,#5953,#5954,
#5955,#5956,#5957,#5958,#5959,#5960,#5961,#5962,#5963,#5964,#5965,#5966,
#5967,#5968));
#6103=CLOSED_SHELL('',(#5969,#5970,#5971,#5972));
#6104=CLOSED_SHELL('',(#5973,#5974,#5975,#5976,#5977,#5978,#5979));
#6105=CLOSED_SHELL('',(#5980,#5981,#5982,#5983,#5984,#5985,#5986,#5987,
#5988,#5989,#5990));
#6106=CLOSED_SHELL('',(#5991,#5992,#5993,#5994));
#6107=CLOSED_SHELL('',(#5995,#5996,#5997,#5998));
#6108=CLOSED_SHELL('',(#5999,#6000,#6001,#6002));
#6109=CLOSED_SHELL('',(#6003,#6004,#6005,#6006));
#6110=CLOSED_SHELL('',(#6007,#6008,#6009,#6010,#6011,#6012,#6013,#6014,
#6015,#6016,#6017));
#6111=CLOSED_SHELL('',(#6018,#6019,#6020,#6021,#6022,#6023,#6024,#6025,
#6026));
#6112=CLOSED_SHELL('',(#6027,#6028,#6029,#6030,#6031,#6032,#6033,#6034));
#6113=CLOSED_SHELL('',(#6035,#6036,#6037,#6038,#6039,#6040,#6041,#6042));
#6114=CLOSED_SHELL('',(#6043,#6044,#6045,#6046,#6047,#6048,#6049,#6050));
#6115=CLOSED_SHELL('',(#6051,#6052,#6053,#6054,#6055,#6056,#6057,#6058));
#6116=CLOSED_SHELL('',(#6059,#6060,#6061,#6062));
#6117=CLOSED_SHELL('',(#6063,#6064,#6065,#6066));
#6118=DERIVED_UNIT_ELEMENT(#6198,1.);
#6119=DERIVED_UNIT_ELEMENT(#11918,-3.);
#6120=DERIVED_UNIT_ELEMENT(#6198,1.);
#6121=DERIVED_UNIT_ELEMENT(#11918,-3.);
#6122=DERIVED_UNIT_ELEMENT(#6198,1.);
#6123=DERIVED_UNIT_ELEMENT(#11918,-3.);
#6124=DERIVED_UNIT_ELEMENT(#6198,1.);
#6125=DERIVED_UNIT_ELEMENT(#11918,-3.);
#6126=DERIVED_UNIT_ELEMENT(#6198,1.);
#6127=DERIVED_UNIT_ELEMENT(#11918,-3.);
#6128=DERIVED_UNIT_ELEMENT(#6198,1.);
#6129=DERIVED_UNIT_ELEMENT(#11918,-3.);
#6130=DERIVED_UNIT_ELEMENT(#6198,1.);
#6131=DERIVED_UNIT_ELEMENT(#11918,-3.);
#6132=DERIVED_UNIT_ELEMENT(#6198,1.);
#6133=DERIVED_UNIT_ELEMENT(#11918,-3.);
#6134=DERIVED_UNIT_ELEMENT(#6198,1.);
#6135=DERIVED_UNIT_ELEMENT(#11918,-3.);
#6136=DERIVED_UNIT_ELEMENT(#6198,1.);
#6137=DERIVED_UNIT_ELEMENT(#11918,-3.);
#6138=DERIVED_UNIT_ELEMENT(#6198,1.);
#6139=DERIVED_UNIT_ELEMENT(#11918,-3.);
#6140=DERIVED_UNIT_ELEMENT(#6198,1.);
#6141=DERIVED_UNIT_ELEMENT(#11918,-3.);
#6142=DERIVED_UNIT_ELEMENT(#6198,1.);
#6143=DERIVED_UNIT_ELEMENT(#11918,-3.);
#6144=DERIVED_UNIT_ELEMENT(#6198,1.);
#6145=DERIVED_UNIT_ELEMENT(#11918,-3.);
#6146=DERIVED_UNIT_ELEMENT(#6198,1.);
#6147=DERIVED_UNIT_ELEMENT(#11918,-3.);
#6148=DERIVED_UNIT_ELEMENT(#6198,1.);
#6149=DERIVED_UNIT_ELEMENT(#11918,-3.);
#6150=DERIVED_UNIT_ELEMENT(#6198,1.);
#6151=DERIVED_UNIT_ELEMENT(#11918,-3.);
#6152=DERIVED_UNIT_ELEMENT(#6198,1.);
#6153=DERIVED_UNIT_ELEMENT(#11918,-3.);
#6154=DERIVED_UNIT_ELEMENT(#6198,1.);
#6155=DERIVED_UNIT_ELEMENT(#11918,-3.);
#6156=DERIVED_UNIT_ELEMENT(#6198,1.);
#6157=DERIVED_UNIT_ELEMENT(#11918,-3.);
#6158=DERIVED_UNIT_ELEMENT(#6198,1.);
#6159=DERIVED_UNIT_ELEMENT(#11918,-3.);
#6160=DERIVED_UNIT_ELEMENT(#6198,1.);
#6161=DERIVED_UNIT_ELEMENT(#11918,-3.);
#6162=DERIVED_UNIT_ELEMENT(#6198,1.);
#6163=DERIVED_UNIT_ELEMENT(#11918,-3.);
#6164=DERIVED_UNIT_ELEMENT(#6198,1.);
#6165=DERIVED_UNIT_ELEMENT(#11918,-3.);
#6166=DERIVED_UNIT_ELEMENT(#6198,1.);
#6167=DERIVED_UNIT_ELEMENT(#11918,-3.);
#6168=DERIVED_UNIT_ELEMENT(#6198,1.);
#6169=DERIVED_UNIT_ELEMENT(#11918,-3.);
#6170=DERIVED_UNIT_ELEMENT(#6198,1.);
#6171=DERIVED_UNIT_ELEMENT(#11918,-3.);
#6172=DERIVED_UNIT_ELEMENT(#6198,1.);
#6173=DERIVED_UNIT_ELEMENT(#11918,-3.);
#6174=DERIVED_UNIT_ELEMENT(#6198,1.);
#6175=DERIVED_UNIT_ELEMENT(#11918,-3.);
#6176=DERIVED_UNIT_ELEMENT(#6198,1.);
#6177=DERIVED_UNIT_ELEMENT(#11918,-3.);
#6178=DERIVED_UNIT_ELEMENT(#6198,1.);
#6179=DERIVED_UNIT_ELEMENT(#11918,-3.);
#6180=DERIVED_UNIT_ELEMENT(#6198,1.);
#6181=DERIVED_UNIT_ELEMENT(#11918,-3.);
#6182=DERIVED_UNIT_ELEMENT(#6198,1.);
#6183=DERIVED_UNIT_ELEMENT(#11918,-3.);
#6184=DERIVED_UNIT_ELEMENT(#6198,1.);
#6185=DERIVED_UNIT_ELEMENT(#11918,-3.);
#6186=DERIVED_UNIT_ELEMENT(#6198,1.);
#6187=DERIVED_UNIT_ELEMENT(#11918,-3.);
#6188=DERIVED_UNIT_ELEMENT(#6198,1.);
#6189=DERIVED_UNIT_ELEMENT(#11918,-3.);
#6190=DERIVED_UNIT_ELEMENT(#6198,1.);
#6191=DERIVED_UNIT_ELEMENT(#11918,-3.);
#6192=DERIVED_UNIT_ELEMENT(#6198,1.);
#6193=DERIVED_UNIT_ELEMENT(#11918,-3.);
#6194=DERIVED_UNIT_ELEMENT(#6198,1.);
#6195=DERIVED_UNIT_ELEMENT(#11918,-3.);
#6196=DERIVED_UNIT_ELEMENT(#6198,1.);
#6197=DERIVED_UNIT_ELEMENT(#11918,-3.);
#6198=(
MASS_UNIT()
NAMED_UNIT(*)
SI_UNIT(.KILO.,.GRAM.)
);
#6199=DERIVED_UNIT((#6118,#6119));
#6200=DERIVED_UNIT((#6120,#6121));
#6201=DERIVED_UNIT((#6122,#6123));
#6202=DERIVED_UNIT((#6124,#6125));
#6203=DERIVED_UNIT((#6126,#6127));
#6204=DERIVED_UNIT((#6128,#6129));
#6205=DERIVED_UNIT((#6130,#6131));
#6206=DERIVED_UNIT((#6132,#6133));
#6207=DERIVED_UNIT((#6134,#6135));
#6208=DERIVED_UNIT((#6136,#6137));
#6209=DERIVED_UNIT((#6138,#6139));
#6210=DERIVED_UNIT((#6140,#6141));
#6211=DERIVED_UNIT((#6142,#6143));
#6212=DERIVED_UNIT((#6144,#6145));
#6213=DERIVED_UNIT((#6146,#6147));
#6214=DERIVED_UNIT((#6148,#6149));
#6215=DERIVED_UNIT((#6150,#6151));
#6216=DERIVED_UNIT((#6152,#6153));
#6217=DERIVED_UNIT((#6154,#6155));
#6218=DERIVED_UNIT((#6156,#6157));
#6219=DERIVED_UNIT((#6158,#6159));
#6220=DERIVED_UNIT((#6160,#6161));
#6221=DERIVED_UNIT((#6162,#6163));
#6222=DERIVED_UNIT((#6164,#6165));
#6223=DERIVED_UNIT((#6166,#6167));
#6224=DERIVED_UNIT((#6168,#6169));
#6225=DERIVED_UNIT((#6170,#6171));
#6226=DERIVED_UNIT((#6172,#6173));
#6227=DERIVED_UNIT((#6174,#6175));
#6228=DERIVED_UNIT((#6176,#6177));
#6229=DERIVED_UNIT((#6178,#6179));
#6230=DERIVED_UNIT((#6180,#6181));
#6231=DERIVED_UNIT((#6182,#6183));
#6232=DERIVED_UNIT((#6184,#6185));
#6233=DERIVED_UNIT((#6186,#6187));
#6234=DERIVED_UNIT((#6188,#6189));
#6235=DERIVED_UNIT((#6190,#6191));
#6236=DERIVED_UNIT((#6192,#6193));
#6237=DERIVED_UNIT((#6194,#6195));
#6238=DERIVED_UNIT((#6196,#6197));
#6239=MEASURE_REPRESENTATION_ITEM('density measure',
POSITIVE_RATIO_MEASURE(7850.),#6199);
#6240=MEASURE_REPRESENTATION_ITEM('density measure',
POSITIVE_RATIO_MEASURE(7850.),#6200);
#6241=MEASURE_REPRESENTATION_ITEM('density measure',
POSITIVE_RATIO_MEASURE(7850.),#6201);
#6242=MEASURE_REPRESENTATION_ITEM('density measure',
POSITIVE_RATIO_MEASURE(7850.),#6202);
#6243=MEASURE_REPRESENTATION_ITEM('density measure',
POSITIVE_RATIO_MEASURE(7850.),#6203);
#6244=MEASURE_REPRESENTATION_ITEM('density measure',
POSITIVE_RATIO_MEASURE(7850.),#6204);
#6245=MEASURE_REPRESENTATION_ITEM('density measure',
POSITIVE_RATIO_MEASURE(7850.),#6205);
#6246=MEASURE_REPRESENTATION_ITEM('density measure',
POSITIVE_RATIO_MEASURE(7850.),#6206);
#6247=MEASURE_REPRESENTATION_ITEM('density measure',
POSITIVE_RATIO_MEASURE(7850.),#6207);
#6248=MEASURE_REPRESENTATION_ITEM('density measure',
POSITIVE_RATIO_MEASURE(7850.),#6208);
#6249=MEASURE_REPRESENTATION_ITEM('density measure',
POSITIVE_RATIO_MEASURE(7850.),#6209);
#6250=MEASURE_REPRESENTATION_ITEM('density measure',
POSITIVE_RATIO_MEASURE(7850.),#6210);
#6251=MEASURE_REPRESENTATION_ITEM('density measure',
POSITIVE_RATIO_MEASURE(7850.),#6211);
#6252=MEASURE_REPRESENTATION_ITEM('density measure',
POSITIVE_RATIO_MEASURE(7850.),#6212);
#6253=MEASURE_REPRESENTATION_ITEM('density measure',
POSITIVE_RATIO_MEASURE(7850.),#6213);
#6254=MEASURE_REPRESENTATION_ITEM('density measure',
POSITIVE_RATIO_MEASURE(7850.),#6214);
#6255=MEASURE_REPRESENTATION_ITEM('density measure',
POSITIVE_RATIO_MEASURE(7850.),#6215);
#6256=MEASURE_REPRESENTATION_ITEM('density measure',
POSITIVE_RATIO_MEASURE(7850.),#6216);
#6257=MEASURE_REPRESENTATION_ITEM('density measure',
POSITIVE_RATIO_MEASURE(7850.),#6217);
#6258=MEASURE_REPRESENTATION_ITEM('density measure',
POSITIVE_RATIO_MEASURE(7850.),#6218);
#6259=MEASURE_REPRESENTATION_ITEM('density measure',
POSITIVE_RATIO_MEASURE(7850.),#6219);
#6260=MEASURE_REPRESENTATION_ITEM('density measure',
POSITIVE_RATIO_MEASURE(7850.),#6220);
#6261=MEASURE_REPRESENTATION_ITEM('density measure',
POSITIVE_RATIO_MEASURE(7850.),#6221);
#6262=MEASURE_REPRESENTATION_ITEM('density measure',
POSITIVE_RATIO_MEASURE(7850.),#6222);
#6263=MEASURE_REPRESENTATION_ITEM('density measure',
POSITIVE_RATIO_MEASURE(7850.),#6223);
#6264=MEASURE_REPRESENTATION_ITEM('density measure',
POSITIVE_RATIO_MEASURE(7850.),#6224);
#6265=MEASURE_REPRESENTATION_ITEM('density measure',
POSITIVE_RATIO_MEASURE(7850.),#6225);
#6266=MEASURE_REPRESENTATION_ITEM('density measure',
POSITIVE_RATIO_MEASURE(7850.),#6226);
#6267=MEASURE_REPRESENTATION_ITEM('density measure',
POSITIVE_RATIO_MEASURE(7850.),#6227);
#6268=MEASURE_REPRESENTATION_ITEM('density measure',
POSITIVE_RATIO_MEASURE(7850.),#6228);
#6269=MEASURE_REPRESENTATION_ITEM('density measure',
POSITIVE_RATIO_MEASURE(7850.),#6229);
#6270=MEASURE_REPRESENTATION_ITEM('density measure',
POSITIVE_RATIO_MEASURE(7850.),#6230);
#6271=MEASURE_REPRESENTATION_ITEM('density measure',
POSITIVE_RATIO_MEASURE(7850.),#6231);
#6272=MEASURE_REPRESENTATION_ITEM('density measure',
POSITIVE_RATIO_MEASURE(7850.),#6232);
#6273=MEASURE_REPRESENTATION_ITEM('density measure',
POSITIVE_RATIO_MEASURE(7850.),#6233);
#6274=MEASURE_REPRESENTATION_ITEM('density measure',
POSITIVE_RATIO_MEASURE(7850.),#6234);
#6275=MEASURE_REPRESENTATION_ITEM('density measure',
POSITIVE_RATIO_MEASURE(7850.),#6235);
#6276=MEASURE_REPRESENTATION_ITEM('density measure',
POSITIVE_RATIO_MEASURE(7850.),#6236);
#6277=MEASURE_REPRESENTATION_ITEM('density measure',
POSITIVE_RATIO_MEASURE(7850.),#6237);
#6278=MEASURE_REPRESENTATION_ITEM('density measure',
POSITIVE_RATIO_MEASURE(7850.),#6238);
#6279=PROPERTY_DEFINITION_REPRESENTATION(#6479,#6359);
#6280=PROPERTY_DEFINITION_REPRESENTATION(#6480,#6360);
#6281=PROPERTY_DEFINITION_REPRESENTATION(#6481,#6361);
#6282=PROPERTY_DEFINITION_REPRESENTATION(#6482,#6362);
#6283=PROPERTY_DEFINITION_REPRESENTATION(#6483,#6363);
#6284=PROPERTY_DEFINITION_REPRESENTATION(#6484,#6364);
#6285=PROPERTY_DEFINITION_REPRESENTATION(#6485,#6365);
#6286=PROPERTY_DEFINITION_REPRESENTATION(#6486,#6366);
#6287=PROPERTY_DEFINITION_REPRESENTATION(#6487,#6367);
#6288=PROPERTY_DEFINITION_REPRESENTATION(#6488,#6368);
#6289=PROPERTY_DEFINITION_REPRESENTATION(#6489,#6369);
#6290=PROPERTY_DEFINITION_REPRESENTATION(#6490,#6370);
#6291=PROPERTY_DEFINITION_REPRESENTATION(#6491,#6371);
#6292=PROPERTY_DEFINITION_REPRESENTATION(#6492,#6372);
#6293=PROPERTY_DEFINITION_REPRESENTATION(#6493,#6373);
#6294=PROPERTY_DEFINITION_REPRESENTATION(#6494,#6374);
#6295=PROPERTY_DEFINITION_REPRESENTATION(#6495,#6375);
#6296=PROPERTY_DEFINITION_REPRESENTATION(#6496,#6376);
#6297=PROPERTY_DEFINITION_REPRESENTATION(#6497,#6377);
#6298=PROPERTY_DEFINITION_REPRESENTATION(#6498,#6378);
#6299=PROPERTY_DEFINITION_REPRESENTATION(#6499,#6379);
#6300=PROPERTY_DEFINITION_REPRESENTATION(#6500,#6380);
#6301=PROPERTY_DEFINITION_REPRESENTATION(#6501,#6381);
#6302=PROPERTY_DEFINITION_REPRESENTATION(#6502,#6382);
#6303=PROPERTY_DEFINITION_REPRESENTATION(#6503,#6383);
#6304=PROPERTY_DEFINITION_REPRESENTATION(#6504,#6384);
#6305=PROPERTY_DEFINITION_REPRESENTATION(#6505,#6385);
#6306=PROPERTY_DEFINITION_REPRESENTATION(#6506,#6386);
#6307=PROPERTY_DEFINITION_REPRESENTATION(#6507,#6387);
#6308=PROPERTY_DEFINITION_REPRESENTATION(#6508,#6388);
#6309=PROPERTY_DEFINITION_REPRESENTATION(#6509,#6389);
#6310=PROPERTY_DEFINITION_REPRESENTATION(#6510,#6390);
#6311=PROPERTY_DEFINITION_REPRESENTATION(#6511,#6391);
#6312=PROPERTY_DEFINITION_REPRESENTATION(#6512,#6392);
#6313=PROPERTY_DEFINITION_REPRESENTATION(#6513,#6393);
#6314=PROPERTY_DEFINITION_REPRESENTATION(#6514,#6394);
#6315=PROPERTY_DEFINITION_REPRESENTATION(#6515,#6395);
#6316=PROPERTY_DEFINITION_REPRESENTATION(#6516,#6396);
#6317=PROPERTY_DEFINITION_REPRESENTATION(#6517,#6397);
#6318=PROPERTY_DEFINITION_REPRESENTATION(#6518,#6398);
#6319=PROPERTY_DEFINITION_REPRESENTATION(#6519,#6399);
#6320=PROPERTY_DEFINITION_REPRESENTATION(#6520,#6400);
#6321=PROPERTY_DEFINITION_REPRESENTATION(#6521,#6401);
#6322=PROPERTY_DEFINITION_REPRESENTATION(#6522,#6402);
#6323=PROPERTY_DEFINITION_REPRESENTATION(#6523,#6403);
#6324=PROPERTY_DEFINITION_REPRESENTATION(#6524,#6404);
#6325=PROPERTY_DEFINITION_REPRESENTATION(#6525,#6405);
#6326=PROPERTY_DEFINITION_REPRESENTATION(#6526,#6406);
#6327=PROPERTY_DEFINITION_REPRESENTATION(#6527,#6407);
#6328=PROPERTY_DEFINITION_REPRESENTATION(#6528,#6408);
#6329=PROPERTY_DEFINITION_REPRESENTATION(#6529,#6409);
#6330=PROPERTY_DEFINITION_REPRESENTATION(#6530,#6410);
#6331=PROPERTY_DEFINITION_REPRESENTATION(#6531,#6411);
#6332=PROPERTY_DEFINITION_REPRESENTATION(#6532,#6412);
#6333=PROPERTY_DEFINITION_REPRESENTATION(#6533,#6413);
#6334=PROPERTY_DEFINITION_REPRESENTATION(#6534,#6414);
#6335=PROPERTY_DEFINITION_REPRESENTATION(#6535,#6415);
#6336=PROPERTY_DEFINITION_REPRESENTATION(#6536,#6416);
#6337=PROPERTY_DEFINITION_REPRESENTATION(#6537,#6417);
#6338=PROPERTY_DEFINITION_REPRESENTATION(#6538,#6418);
#6339=PROPERTY_DEFINITION_REPRESENTATION(#6539,#6419);
#6340=PROPERTY_DEFINITION_REPRESENTATION(#6540,#6420);
#6341=PROPERTY_DEFINITION_REPRESENTATION(#6541,#6421);
#6342=PROPERTY_DEFINITION_REPRESENTATION(#6542,#6422);
#6343=PROPERTY_DEFINITION_REPRESENTATION(#6543,#6423);
#6344=PROPERTY_DEFINITION_REPRESENTATION(#6544,#6424);
#6345=PROPERTY_DEFINITION_REPRESENTATION(#6545,#6425);
#6346=PROPERTY_DEFINITION_REPRESENTATION(#6546,#6426);
#6347=PROPERTY_DEFINITION_REPRESENTATION(#6547,#6427);
#6348=PROPERTY_DEFINITION_REPRESENTATION(#6548,#6428);
#6349=PROPERTY_DEFINITION_REPRESENTATION(#6549,#6429);
#6350=PROPERTY_DEFINITION_REPRESENTATION(#6550,#6430);
#6351=PROPERTY_DEFINITION_REPRESENTATION(#6551,#6431);
#6352=PROPERTY_DEFINITION_REPRESENTATION(#6552,#6432);
#6353=PROPERTY_DEFINITION_REPRESENTATION(#6553,#6433);
#6354=PROPERTY_DEFINITION_REPRESENTATION(#6554,#6434);
#6355=PROPERTY_DEFINITION_REPRESENTATION(#6555,#6435);
#6356=PROPERTY_DEFINITION_REPRESENTATION(#6556,#6436);
#6357=PROPERTY_DEFINITION_REPRESENTATION(#6557,#6437);
#6358=PROPERTY_DEFINITION_REPRESENTATION(#6558,#6438);
#6359=REPRESENTATION('material name',(#6439),#11872);
#6360=REPRESENTATION('density',(#6239),#11872);
#6361=REPRESENTATION('material name',(#6440),#11873);
#6362=REPRESENTATION('density',(#6240),#11873);
#6363=REPRESENTATION('material name',(#6441),#11874);
#6364=REPRESENTATION('density',(#6241),#11874);
#6365=REPRESENTATION('material name',(#6442),#11875);
#6366=REPRESENTATION('density',(#6242),#11875);
#6367=REPRESENTATION('material name',(#6443),#11876);
#6368=REPRESENTATION('density',(#6243),#11876);
#6369=REPRESENTATION('material name',(#6444),#11877);
#6370=REPRESENTATION('density',(#6244),#11877);
#6371=REPRESENTATION('material name',(#6445),#11878);
#6372=REPRESENTATION('density',(#6245),#11878);
#6373=REPRESENTATION('material name',(#6446),#11879);
#6374=REPRESENTATION('density',(#6246),#11879);
#6375=REPRESENTATION('material name',(#6447),#11880);
#6376=REPRESENTATION('density',(#6247),#11880);
#6377=REPRESENTATION('material name',(#6448),#11882);
#6378=REPRESENTATION('density',(#6248),#11882);
#6379=REPRESENTATION('material name',(#6449),#11883);
#6380=REPRESENTATION('density',(#6249),#11883);
#6381=REPRESENTATION('material name',(#6450),#11884);
#6382=REPRESENTATION('density',(#6250),#11884);
#6383=REPRESENTATION('material name',(#6451),#11885);
#6384=REPRESENTATION('density',(#6251),#11885);
#6385=REPRESENTATION('material name',(#6452),#11886);
#6386=REPRESENTATION('density',(#6252),#11886);
#6387=REPRESENTATION('material name',(#6453),#11888);
#6388=REPRESENTATION('density',(#6253),#11888);
#6389=REPRESENTATION('material name',(#6454),#11889);
#6390=REPRESENTATION('density',(#6254),#11889);
#6391=REPRESENTATION('material name',(#6455),#11890);
#6392=REPRESENTATION('density',(#6255),#11890);
#6393=REPRESENTATION('material name',(#6456),#11891);
#6394=REPRESENTATION('density',(#6256),#11891);
#6395=REPRESENTATION('material name',(#6457),#11892);
#6396=REPRESENTATION('density',(#6257),#11892);
#6397=REPRESENTATION('material name',(#6458),#11893);
#6398=REPRESENTATION('density',(#6258),#11893);
#6399=REPRESENTATION('material name',(#6459),#11894);
#6400=REPRESENTATION('density',(#6259),#11894);
#6401=REPRESENTATION('material name',(#6460),#11895);
#6402=REPRESENTATION('density',(#6260),#11895);
#6403=REPRESENTATION('material name',(#6461),#11896);
#6404=REPRESENTATION('density',(#6261),#11896);
#6405=REPRESENTATION('material name',(#6462),#11897);
#6406=REPRESENTATION('density',(#6262),#11897);
#6407=REPRESENTATION('material name',(#6463),#11898);
#6408=REPRESENTATION('density',(#6263),#11898);
#6409=REPRESENTATION('material name',(#6464),#11899);
#6410=REPRESENTATION('density',(#6264),#11899);
#6411=REPRESENTATION('material name',(#6465),#11901);
#6412=REPRESENTATION('density',(#6265),#11901);
#6413=REPRESENTATION('material name',(#6466),#11902);
#6414=REPRESENTATION('density',(#6266),#11902);
#6415=REPRESENTATION('material name',(#6467),#11903);
#6416=REPRESENTATION('density',(#6267),#11903);
#6417=REPRESENTATION('material name',(#6468),#11904);
#6418=REPRESENTATION('density',(#6268),#11904);
#6419=REPRESENTATION('material name',(#6469),#11905);
#6420=REPRESENTATION('density',(#6269),#11905);
#6421=REPRESENTATION('material name',(#6470),#11906);
#6422=REPRESENTATION('density',(#6270),#11906);
#6423=REPRESENTATION('material name',(#6471),#11907);
#6424=REPRESENTATION('density',(#6271),#11907);
#6425=REPRESENTATION('material name',(#6472),#11908);
#6426=REPRESENTATION('density',(#6272),#11908);
#6427=REPRESENTATION('material name',(#6473),#11909);
#6428=REPRESENTATION('density',(#6273),#11909);
#6429=REPRESENTATION('material name',(#6474),#11910);
#6430=REPRESENTATION('density',(#6274),#11910);
#6431=REPRESENTATION('material name',(#6475),#11911);
#6432=REPRESENTATION('density',(#6275),#11911);
#6433=REPRESENTATION('material name',(#6476),#11913);
#6434=REPRESENTATION('density',(#6276),#11913);
#6435=REPRESENTATION('material name',(#6477),#11914);
#6436=REPRESENTATION('density',(#6277),#11914);
#6437=REPRESENTATION('material name',(#6478),#11915);
#6438=REPRESENTATION('density',(#6278),#11915);
#6439=DESCRIPTIVE_REPRESENTATION_ITEM('Steel','Steel');
#6440=DESCRIPTIVE_REPRESENTATION_ITEM('Steel','Steel');
#6441=DESCRIPTIVE_REPRESENTATION_ITEM('Steel','Steel');
#6442=DESCRIPTIVE_REPRESENTATION_ITEM('Steel','Steel');
#6443=DESCRIPTIVE_REPRESENTATION_ITEM('Steel','Steel');
#6444=DESCRIPTIVE_REPRESENTATION_ITEM('Steel','Steel');
#6445=DESCRIPTIVE_REPRESENTATION_ITEM('Steel','Steel');
#6446=DESCRIPTIVE_REPRESENTATION_ITEM('Steel','Steel');
#6447=DESCRIPTIVE_REPRESENTATION_ITEM('Steel','Steel');
#6448=DESCRIPTIVE_REPRESENTATION_ITEM('Steel','Steel');
#6449=DESCRIPTIVE_REPRESENTATION_ITEM('Steel','Steel');
#6450=DESCRIPTIVE_REPRESENTATION_ITEM('Steel','Steel');
#6451=DESCRIPTIVE_REPRESENTATION_ITEM('Steel','Steel');
#6452=DESCRIPTIVE_REPRESENTATION_ITEM('Steel','Steel');
#6453=DESCRIPTIVE_REPRESENTATION_ITEM('Steel','Steel');
#6454=DESCRIPTIVE_REPRESENTATION_ITEM('Steel','Steel');
#6455=DESCRIPTIVE_REPRESENTATION_ITEM('Steel','Steel');
#6456=DESCRIPTIVE_REPRESENTATION_ITEM('Steel','Steel');
#6457=DESCRIPTIVE_REPRESENTATION_ITEM('Steel','Steel');
#6458=DESCRIPTIVE_REPRESENTATION_ITEM('Steel','Steel');
#6459=DESCRIPTIVE_REPRESENTATION_ITEM('Steel','Steel');
#6460=DESCRIPTIVE_REPRESENTATION_ITEM('Steel','Steel');
#6461=DESCRIPTIVE_REPRESENTATION_ITEM('Steel','Steel');
#6462=DESCRIPTIVE_REPRESENTATION_ITEM('Steel','Steel');
#6463=DESCRIPTIVE_REPRESENTATION_ITEM('Steel','Steel');
#6464=DESCRIPTIVE_REPRESENTATION_ITEM('Steel','Steel');
#6465=DESCRIPTIVE_REPRESENTATION_ITEM('Steel','Steel');
#6466=DESCRIPTIVE_REPRESENTATION_ITEM('Steel','Steel');
#6467=DESCRIPTIVE_REPRESENTATION_ITEM('Steel','Steel');
#6468=DESCRIPTIVE_REPRESENTATION_ITEM('Steel','Steel');
#6469=DESCRIPTIVE_REPRESENTATION_ITEM('Steel','Steel');
#6470=DESCRIPTIVE_REPRESENTATION_ITEM('Steel','Steel');
#6471=DESCRIPTIVE_REPRESENTATION_ITEM('Steel','Steel');
#6472=DESCRIPTIVE_REPRESENTATION_ITEM('Steel','Steel');
#6473=DESCRIPTIVE_REPRESENTATION_ITEM('Steel','Steel');
#6474=DESCRIPTIVE_REPRESENTATION_ITEM('Steel','Steel');
#6475=DESCRIPTIVE_REPRESENTATION_ITEM('Steel','Steel');
#6476=DESCRIPTIVE_REPRESENTATION_ITEM('Steel','Steel');
#6477=DESCRIPTIVE_REPRESENTATION_ITEM('Steel','Steel');
#6478=DESCRIPTIVE_REPRESENTATION_ITEM('Steel','Steel');
#6479=PROPERTY_DEFINITION('material property','material name',#12128);
#6480=PROPERTY_DEFINITION('material property','density of part',#12128);
#6481=PROPERTY_DEFINITION('material property','material name',#12129);
#6482=PROPERTY_DEFINITION('material property','density of part',#12129);
#6483=PROPERTY_DEFINITION('material property','material name',#12130);
#6484=PROPERTY_DEFINITION('material property','density of part',#12130);
#6485=PROPERTY_DEFINITION('material property','material name',#12131);
#6486=PROPERTY_DEFINITION('material property','density of part',#12131);
#6487=PROPERTY_DEFINITION('material property','material name',#12132);
#6488=PROPERTY_DEFINITION('material property','density of part',#12132);
#6489=PROPERTY_DEFINITION('material property','material name',#12133);
#6490=PROPERTY_DEFINITION('material property','density of part',#12133);
#6491=PROPERTY_DEFINITION('material property','material name',#12134);
#6492=PROPERTY_DEFINITION('material property','density of part',#12134);
#6493=PROPERTY_DEFINITION('material property','material name',#12135);
#6494=PROPERTY_DEFINITION('material property','density of part',#12135);
#6495=PROPERTY_DEFINITION('material property','material name',#12136);
#6496=PROPERTY_DEFINITION('material property','density of part',#12136);
#6497=PROPERTY_DEFINITION('material property','material name',#12138);
#6498=PROPERTY_DEFINITION('material property','density of part',#12138);
#6499=PROPERTY_DEFINITION('material property','material name',#12139);
#6500=PROPERTY_DEFINITION('material property','density of part',#12139);
#6501=PROPERTY_DEFINITION('material property','material name',#12140);
#6502=PROPERTY_DEFINITION('material property','density of part',#12140);
#6503=PROPERTY_DEFINITION('material property','material name',#12141);
#6504=PROPERTY_DEFINITION('material property','density of part',#12141);
#6505=PROPERTY_DEFINITION('material property','material name',#12142);
#6506=PROPERTY_DEFINITION('material property','density of part',#12142);
#6507=PROPERTY_DEFINITION('material property','material name',#12144);
#6508=PROPERTY_DEFINITION('material property','density of part',#12144);
#6509=PROPERTY_DEFINITION('material property','material name',#12145);
#6510=PROPERTY_DEFINITION('material property','density of part',#12145);
#6511=PROPERTY_DEFINITION('material property','material name',#12146);
#6512=PROPERTY_DEFINITION('material property','density of part',#12146);
#6513=PROPERTY_DEFINITION('material property','material name',#12147);
#6514=PROPERTY_DEFINITION('material property','density of part',#12147);
#6515=PROPERTY_DEFINITION('material property','material name',#12148);
#6516=PROPERTY_DEFINITION('material property','density of part',#12148);
#6517=PROPERTY_DEFINITION('material property','material name',#12149);
#6518=PROPERTY_DEFINITION('material property','density of part',#12149);
#6519=PROPERTY_DEFINITION('material property','material name',#12150);
#6520=PROPERTY_DEFINITION('material property','density of part',#12150);
#6521=PROPERTY_DEFINITION('material property','material name',#12151);
#6522=PROPERTY_DEFINITION('material property','density of part',#12151);
#6523=PROPERTY_DEFINITION('material property','material name',#12152);
#6524=PROPERTY_DEFINITION('material property','density of part',#12152);
#6525=PROPERTY_DEFINITION('material property','material name',#12153);
#6526=PROPERTY_DEFINITION('material property','density of part',#12153);
#6527=PROPERTY_DEFINITION('material property','material name',#12154);
#6528=PROPERTY_DEFINITION('material property','density of part',#12154);
#6529=PROPERTY_DEFINITION('material property','material name',#12155);
#6530=PROPERTY_DEFINITION('material property','density of part',#12155);
#6531=PROPERTY_DEFINITION('material property','material name',#12157);
#6532=PROPERTY_DEFINITION('material property','density of part',#12157);
#6533=PROPERTY_DEFINITION('material property','material name',#12158);
#6534=PROPERTY_DEFINITION('material property','density of part',#12158);
#6535=PROPERTY_DEFINITION('material property','material name',#12159);
#6536=PROPERTY_DEFINITION('material property','density of part',#12159);
#6537=PROPERTY_DEFINITION('material property','material name',#12160);
#6538=PROPERTY_DEFINITION('material property','density of part',#12160);
#6539=PROPERTY_DEFINITION('material property','material name',#12161);
#6540=PROPERTY_DEFINITION('material property','density of part',#12161);
#6541=PROPERTY_DEFINITION('material property','material name',#12162);
#6542=PROPERTY_DEFINITION('material property','density of part',#12162);
#6543=PROPERTY_DEFINITION('material property','material name',#12163);
#6544=PROPERTY_DEFINITION('material property','density of part',#12163);
#6545=PROPERTY_DEFINITION('material property','material name',#12164);
#6546=PROPERTY_DEFINITION('material property','density of part',#12164);
#6547=PROPERTY_DEFINITION('material property','material name',#12165);
#6548=PROPERTY_DEFINITION('material property','density of part',#12165);
#6549=PROPERTY_DEFINITION('material property','material name',#12166);
#6550=PROPERTY_DEFINITION('material property','density of part',#12166);
#6551=PROPERTY_DEFINITION('material property','material name',#12167);
#6552=PROPERTY_DEFINITION('material property','density of part',#12167);
#6553=PROPERTY_DEFINITION('material property','material name',#12169);
#6554=PROPERTY_DEFINITION('material property','density of part',#12169);
#6555=PROPERTY_DEFINITION('material property','material name',#12170);
#6556=PROPERTY_DEFINITION('material property','density of part',#12170);
#6557=PROPERTY_DEFINITION('material property','material name',#12171);
#6558=PROPERTY_DEFINITION('material property','density of part',#12171);
#6559=AXIS2_PLACEMENT_3D('',#9448,#7411,#7412);
#6560=AXIS2_PLACEMENT_3D('',#9449,#7413,#7414);
#6561=AXIS2_PLACEMENT_3D('',#9450,#7415,#7416);
#6562=AXIS2_PLACEMENT_3D('',#9451,#7417,#7418);
#6563=AXIS2_PLACEMENT_3D('',#9453,#7419,#7420);
#6564=AXIS2_PLACEMENT_3D('',#9456,#7422,#7423);
#6565=AXIS2_PLACEMENT_3D('',#9457,#7424,#7425);
#6566=AXIS2_PLACEMENT_3D('',#9459,#7426,#7427);
#6567=AXIS2_PLACEMENT_3D('',#9462,#7429,#7430);
#6568=AXIS2_PLACEMENT_3D('',#9463,#7431,#7432);
#6569=AXIS2_PLACEMENT_3D('',#9465,#7433,#7434);
#6570=AXIS2_PLACEMENT_3D('',#9468,#7436,#7437);
#6571=AXIS2_PLACEMENT_3D('',#9469,#7438,#7439);
#6572=AXIS2_PLACEMENT_3D('',#9471,#7440,#7441);
#6573=AXIS2_PLACEMENT_3D('',#9474,#7443,#7444);
#6574=AXIS2_PLACEMENT_3D('',#9475,#7445,#7446);
#6575=AXIS2_PLACEMENT_3D('',#9477,#7447,#7448);
#6576=AXIS2_PLACEMENT_3D('',#9480,#7450,#7451);
#6577=AXIS2_PLACEMENT_3D('',#9481,#7452,#7453);
#6578=AXIS2_PLACEMENT_3D('',#9483,#7454,#7455);
#6579=AXIS2_PLACEMENT_3D('',#9486,#7457,#7458);
#6580=AXIS2_PLACEMENT_3D('',#9487,#7459,#7460);
#6581=AXIS2_PLACEMENT_3D('',#9489,#7461,#7462);
#6582=AXIS2_PLACEMENT_3D('',#9492,#7464,#7465);
#6583=AXIS2_PLACEMENT_3D('',#9493,#7466,#7467);
#6584=AXIS2_PLACEMENT_3D('',#9495,#7468,#7469);
#6585=AXIS2_PLACEMENT_3D('',#9498,#7471,#7472);
#6586=AXIS2_PLACEMENT_3D('',#9499,#7473,#7474);
#6587=AXIS2_PLACEMENT_3D('',#9508,#7479,#7480);
#6588=AXIS2_PLACEMENT_3D('',#9514,#7484,#7485);
#6589=AXIS2_PLACEMENT_3D('',#9520,#7489,#7490);
#6590=AXIS2_PLACEMENT_3D('',#9523,#7493,#7494);
#6591=AXIS2_PLACEMENT_3D('',#9524,#7495,#7496);
#6592=AXIS2_PLACEMENT_3D('',#9525,#7497,#7498);
#6593=AXIS2_PLACEMENT_3D('',#9526,#7499,#7500);
#6594=AXIS2_PLACEMENT_3D('',#9535,#7505,#7506);
#6595=AXIS2_PLACEMENT_3D('',#9541,#7510,#7511);
#6596=AXIS2_PLACEMENT_3D('',#9547,#7515,#7516);
#6597=AXIS2_PLACEMENT_3D('',#9550,#7519,#7520);
#6598=AXIS2_PLACEMENT_3D('',#9551,#7521,#7522);
#6599=AXIS2_PLACEMENT_3D('',#9552,#7523,#7524);
#6600=AXIS2_PLACEMENT_3D('',#9553,#7525,#7526);
#6601=AXIS2_PLACEMENT_3D('',#9562,#7531,#7532);
#6602=AXIS2_PLACEMENT_3D('',#9568,#7536,#7537);
#6603=AXIS2_PLACEMENT_3D('',#9574,#7541,#7542);
#6604=AXIS2_PLACEMENT_3D('',#9577,#7545,#7546);
#6605=AXIS2_PLACEMENT_3D('',#9578,#7547,#7548);
#6606=AXIS2_PLACEMENT_3D('',#9579,#7549,#7550);
#6607=AXIS2_PLACEMENT_3D('',#9580,#7551,#7552);
#6608=AXIS2_PLACEMENT_3D('',#9583,#7553,#7554);
#6609=AXIS2_PLACEMENT_3D('',#9584,#7555,#7556);
#6610=AXIS2_PLACEMENT_3D('',#9585,#7557,#7558);
#6611=AXIS2_PLACEMENT_3D('',#9589,#7560,#7561);
#6612=AXIS2_PLACEMENT_3D('',#9591,#7563,#7564);
#6613=AXIS2_PLACEMENT_3D('',#9596,#7566,#7567);
#6614=AXIS2_PLACEMENT_3D('',#9599,#7569,#7570);
#6615=AXIS2_PLACEMENT_3D('',#9600,#7571,#7572);
#6616=AXIS2_PLACEMENT_3D('',#9601,#7573,#7574);
#6617=AXIS2_PLACEMENT_3D('',#9602,#7575,#7576);
#6618=AXIS2_PLACEMENT_3D('',#9607,#7578,#7579);
#6619=AXIS2_PLACEMENT_3D('',#9610,#7581,#7582);
#6620=AXIS2_PLACEMENT_3D('',#9611,#7583,#7584);
#6621=AXIS2_PLACEMENT_3D('',#9612,#7585,#7586);
#6622=AXIS2_PLACEMENT_3D('',#9613,#7587,#7588);
#6623=AXIS2_PLACEMENT_3D('',#9618,#7590,#7591);
#6624=AXIS2_PLACEMENT_3D('',#9621,#7593,#7594);
#6625=AXIS2_PLACEMENT_3D('',#9622,#7595,#7596);
#6626=AXIS2_PLACEMENT_3D('',#9623,#7597,#7598);
#6627=AXIS2_PLACEMENT_3D('',#9624,#7599,#7600);
#6628=AXIS2_PLACEMENT_3D('',#9626,#7601,#7602);
#6629=AXIS2_PLACEMENT_3D('',#9629,#7604,#7605);
#6630=AXIS2_PLACEMENT_3D('',#9630,#7606,#7607);
#6631=AXIS2_PLACEMENT_3D('',#9631,#7608,#7609);
#6632=AXIS2_PLACEMENT_3D('',#9632,#7610,#7611);
#6633=AXIS2_PLACEMENT_3D('',#9633,#7612,#7613);
#6634=AXIS2_PLACEMENT_3D('',#9634,#7614,#7615);
#6635=AXIS2_PLACEMENT_3D('',#9636,#7616,#7617);
#6636=AXIS2_PLACEMENT_3D('',#9638,#7618,#7619);
#6637=AXIS2_PLACEMENT_3D('',#9640,#7620,#7621);
#6638=AXIS2_PLACEMENT_3D('',#9642,#7622,#7623);
#6639=AXIS2_PLACEMENT_3D('',#9644,#7624,#7625);
#6640=AXIS2_PLACEMENT_3D('',#9645,#7626,#7627);
#6641=AXIS2_PLACEMENT_3D('',#9647,#7628,#7629);
#6642=AXIS2_PLACEMENT_3D('',#9650,#7631,#7632);
#6643=AXIS2_PLACEMENT_3D('',#9651,#7633,#7634);
#6644=AXIS2_PLACEMENT_3D('',#9652,#7635,#7636);
#6645=AXIS2_PLACEMENT_3D('',#9654,#7637,#7638);
#6646=AXIS2_PLACEMENT_3D('',#9657,#7640,#7641);
#6647=AXIS2_PLACEMENT_3D('',#9658,#7642,#7643);
#6648=AXIS2_PLACEMENT_3D('',#9659,#7644,#7645);
#6649=AXIS2_PLACEMENT_3D('',#9661,#7646,#7647);
#6650=AXIS2_PLACEMENT_3D('',#9664,#7649,#7650);
#6651=AXIS2_PLACEMENT_3D('',#9665,#7651,#7652);
#6652=AXIS2_PLACEMENT_3D('',#9666,#7653,#7654);
#6653=AXIS2_PLACEMENT_3D('',#9668,#7655,#7656);
#6654=AXIS2_PLACEMENT_3D('',#9671,#7658,#7659);
#6655=AXIS2_PLACEMENT_3D('',#9672,#7660,#7661);
#6656=AXIS2_PLACEMENT_3D('',#9673,#7662,#7663);
#6657=AXIS2_PLACEMENT_3D('',#9751,#7665,#7666);
#6658=AXIS2_PLACEMENT_3D('',#9753,#7667,#7668);
#6659=AXIS2_PLACEMENT_3D('',#9755,#7670,#7671);
#6660=AXIS2_PLACEMENT_3D('',#9757,#7672,#7673);
#6661=AXIS2_PLACEMENT_3D('',#9759,#7675,#7676);
#6662=AXIS2_PLACEMENT_3D('',#9761,#7677,#7678);
#6663=AXIS2_PLACEMENT_3D('',#9763,#7680,#7681);
#6664=AXIS2_PLACEMENT_3D('',#9765,#7682,#7683);
#6665=AXIS2_PLACEMENT_3D('',#9767,#7685,#7686);
#6666=AXIS2_PLACEMENT_3D('',#9769,#7687,#7688);
#6667=AXIS2_PLACEMENT_3D('',#9772,#7690,#7691);
#6668=AXIS2_PLACEMENT_3D('',#9773,#7692,#7693);
#6669=AXIS2_PLACEMENT_3D('',#9775,#7694,#7695);
#6670=AXIS2_PLACEMENT_3D('',#9776,#7696,#7697);
#6671=AXIS2_PLACEMENT_3D('',#9779,#7699,#7700);
#6672=AXIS2_PLACEMENT_3D('',#9780,#7701,#7702);
#6673=AXIS2_PLACEMENT_3D('',#9783,#7704,#7705);
#6674=AXIS2_PLACEMENT_3D('',#9784,#7706,#7707);
#6675=AXIS2_PLACEMENT_3D('',#9785,#7708,#7709);
#6676=AXIS2_PLACEMENT_3D('',#9786,#7710,#7711);
#6677=AXIS2_PLACEMENT_3D('',#9787,#7712,#7713);
#6678=AXIS2_PLACEMENT_3D('',#9789,#7714,#7715);
#6679=AXIS2_PLACEMENT_3D('',#9792,#7717,#7718);
#6680=AXIS2_PLACEMENT_3D('',#9793,#7719,#7720);
#6681=AXIS2_PLACEMENT_3D('',#9795,#7721,#7722);
#6682=AXIS2_PLACEMENT_3D('',#9798,#7724,#7725);
#6683=AXIS2_PLACEMENT_3D('',#9799,#7726,#7727);
#6684=AXIS2_PLACEMENT_3D('',#9800,#7728,#7729);
#6685=AXIS2_PLACEMENT_3D('',#9801,#7730,#7731);
#6686=AXIS2_PLACEMENT_3D('',#9802,#7732,#7733);
#6687=AXIS2_PLACEMENT_3D('',#9804,#7734,#7735);
#6688=AXIS2_PLACEMENT_3D('',#9807,#7737,#7738);
#6689=AXIS2_PLACEMENT_3D('',#9808,#7739,#7740);
#6690=AXIS2_PLACEMENT_3D('',#9810,#7741,#7742);
#6691=AXIS2_PLACEMENT_3D('',#9813,#7744,#7745);
#6692=AXIS2_PLACEMENT_3D('',#9814,#7746,#7747);
#6693=AXIS2_PLACEMENT_3D('',#9816,#7748,#7749);
#6694=AXIS2_PLACEMENT_3D('',#9819,#7751,#7752);
#6695=AXIS2_PLACEMENT_3D('',#9820,#7753,#7754);
#6696=AXIS2_PLACEMENT_3D('',#9822,#7755,#7756);
#6697=AXIS2_PLACEMENT_3D('',#9825,#7758,#7759);
#6698=AXIS2_PLACEMENT_3D('',#9826,#7760,#7761);
#6699=AXIS2_PLACEMENT_3D('',#9828,#7762,#7763);
#6700=AXIS2_PLACEMENT_3D('',#9831,#7765,#7766);
#6701=AXIS2_PLACEMENT_3D('',#9832,#7767,#7768);
#6702=AXIS2_PLACEMENT_3D('',#9834,#7769,#7770);
#6703=AXIS2_PLACEMENT_3D('',#9835,#7771,#7772);
#6704=AXIS2_PLACEMENT_3D('',#9837,#7773,#7774);
#6705=AXIS2_PLACEMENT_3D('',#9839,#7776,#7777);
#6706=AXIS2_PLACEMENT_3D('',#9841,#7778,#7779);
#6707=AXIS2_PLACEMENT_3D('',#9844,#7781,#7782);
#6708=AXIS2_PLACEMENT_3D('',#9845,#7783,#7784);
#6709=AXIS2_PLACEMENT_3D('',#9846,#7785,#7786);
#6710=AXIS2_PLACEMENT_3D('',#9847,#7787,#7788);
#6711=AXIS2_PLACEMENT_3D('',#9848,#7789,#7790);
#6712=AXIS2_PLACEMENT_3D('',#9851,#7791,#7792);
#6713=AXIS2_PLACEMENT_3D('',#9852,#7793,#7794);
#6714=AXIS2_PLACEMENT_3D('',#9853,#7795,#7796);
#6715=AXIS2_PLACEMENT_3D('',#9857,#7798,#7799);
#6716=AXIS2_PLACEMENT_3D('',#9859,#7801,#7802);
#6717=AXIS2_PLACEMENT_3D('',#9864,#7804,#7805);
#6718=AXIS2_PLACEMENT_3D('',#9867,#7807,#7808);
#6719=AXIS2_PLACEMENT_3D('',#9868,#7809,#7810);
#6720=AXIS2_PLACEMENT_3D('',#9869,#7811,#7812);
#6721=AXIS2_PLACEMENT_3D('',#9870,#7813,#7814);
#6722=AXIS2_PLACEMENT_3D('',#9875,#7816,#7817);
#6723=AXIS2_PLACEMENT_3D('',#9878,#7819,#7820);
#6724=AXIS2_PLACEMENT_3D('',#9879,#7821,#7822);
#6725=AXIS2_PLACEMENT_3D('',#9880,#7823,#7824);
#6726=AXIS2_PLACEMENT_3D('',#9881,#7825,#7826);
#6727=AXIS2_PLACEMENT_3D('',#9886,#7828,#7829);
#6728=AXIS2_PLACEMENT_3D('',#9889,#7831,#7832);
#6729=AXIS2_PLACEMENT_3D('',#9890,#7833,#7834);
#6730=AXIS2_PLACEMENT_3D('',#9891,#7835,#7836);
#6731=AXIS2_PLACEMENT_3D('',#9892,#7837,#7838);
#6732=AXIS2_PLACEMENT_3D('',#9894,#7839,#7840);
#6733=AXIS2_PLACEMENT_3D('',#9897,#7842,#7843);
#6734=AXIS2_PLACEMENT_3D('',#9898,#7844,#7845);
#6735=AXIS2_PLACEMENT_3D('',#9899,#7846,#7847);
#6736=AXIS2_PLACEMENT_3D('',#9900,#7848,#7849);
#6737=AXIS2_PLACEMENT_3D('',#9901,#7850,#7851);
#6738=AXIS2_PLACEMENT_3D('',#9902,#7852,#7853);
#6739=AXIS2_PLACEMENT_3D('',#9904,#7854,#7855);
#6740=AXIS2_PLACEMENT_3D('',#9906,#7856,#7857);
#6741=AXIS2_PLACEMENT_3D('',#9908,#7858,#7859);
#6742=AXIS2_PLACEMENT_3D('',#9910,#7860,#7861);
#6743=AXIS2_PLACEMENT_3D('',#9912,#7862,#7863);
#6744=AXIS2_PLACEMENT_3D('',#9913,#7864,#7865);
#6745=AXIS2_PLACEMENT_3D('',#9915,#7866,#7867);
#6746=AXIS2_PLACEMENT_3D('',#9918,#7869,#7870);
#6747=AXIS2_PLACEMENT_3D('',#9919,#7871,#7872);
#6748=AXIS2_PLACEMENT_3D('',#9920,#7873,#7874);
#6749=AXIS2_PLACEMENT_3D('',#9922,#7875,#7876);
#6750=AXIS2_PLACEMENT_3D('',#9925,#7878,#7879);
#6751=AXIS2_PLACEMENT_3D('',#9926,#7880,#7881);
#6752=AXIS2_PLACEMENT_3D('',#9927,#7882,#7883);
#6753=AXIS2_PLACEMENT_3D('',#9929,#7884,#7885);
#6754=AXIS2_PLACEMENT_3D('',#9932,#7887,#7888);
#6755=AXIS2_PLACEMENT_3D('',#9933,#7889,#7890);
#6756=AXIS2_PLACEMENT_3D('',#9934,#7891,#7892);
#6757=AXIS2_PLACEMENT_3D('',#9936,#7893,#7894);
#6758=AXIS2_PLACEMENT_3D('',#9939,#7896,#7897);
#6759=AXIS2_PLACEMENT_3D('',#9940,#7898,#7899);
#6760=AXIS2_PLACEMENT_3D('',#9941,#7900,#7901);
#6761=AXIS2_PLACEMENT_3D('',#10019,#7903,#7904);
#6762=AXIS2_PLACEMENT_3D('',#10021,#7905,#7906);
#6763=AXIS2_PLACEMENT_3D('',#10023,#7908,#7909);
#6764=AXIS2_PLACEMENT_3D('',#10025,#7910,#7911);
#6765=AXIS2_PLACEMENT_3D('',#10027,#7913,#7914);
#6766=AXIS2_PLACEMENT_3D('',#10029,#7915,#7916);
#6767=AXIS2_PLACEMENT_3D('',#10031,#7918,#7919);
#6768=AXIS2_PLACEMENT_3D('',#10033,#7920,#7921);
#6769=AXIS2_PLACEMENT_3D('',#10035,#7923,#7924);
#6770=AXIS2_PLACEMENT_3D('',#10037,#7925,#7926);
#6771=AXIS2_PLACEMENT_3D('',#10040,#7928,#7929);
#6772=AXIS2_PLACEMENT_3D('',#10041,#7930,#7931);
#6773=AXIS2_PLACEMENT_3D('',#10043,#7932,#7933);
#6774=AXIS2_PLACEMENT_3D('',#10044,#7934,#7935);
#6775=AXIS2_PLACEMENT_3D('',#10047,#7937,#7938);
#6776=AXIS2_PLACEMENT_3D('',#10048,#7939,#7940);
#6777=AXIS2_PLACEMENT_3D('',#10051,#7942,#7943);
#6778=AXIS2_PLACEMENT_3D('',#10052,#7944,#7945);
#6779=AXIS2_PLACEMENT_3D('',#10053,#7946,#7947);
#6780=AXIS2_PLACEMENT_3D('',#10054,#7948,#7949);
#6781=AXIS2_PLACEMENT_3D('',#10055,#7950,#7951);
#6782=AXIS2_PLACEMENT_3D('',#10057,#7952,#7953);
#6783=AXIS2_PLACEMENT_3D('',#10060,#7955,#7956);
#6784=AXIS2_PLACEMENT_3D('',#10061,#7957,#7958);
#6785=AXIS2_PLACEMENT_3D('',#10063,#7959,#7960);
#6786=AXIS2_PLACEMENT_3D('',#10066,#7962,#7963);
#6787=AXIS2_PLACEMENT_3D('',#10067,#7964,#7965);
#6788=AXIS2_PLACEMENT_3D('',#10069,#7966,#7967);
#6789=AXIS2_PLACEMENT_3D('',#10072,#7969,#7970);
#6790=AXIS2_PLACEMENT_3D('',#10073,#7971,#7972);
#6791=AXIS2_PLACEMENT_3D('',#10075,#7973,#7974);
#6792=AXIS2_PLACEMENT_3D('',#10078,#7976,#7977);
#6793=AXIS2_PLACEMENT_3D('',#10079,#7978,#7979);
#6794=AXIS2_PLACEMENT_3D('',#10081,#7980,#7981);
#6795=AXIS2_PLACEMENT_3D('',#10084,#7983,#7984);
#6796=AXIS2_PLACEMENT_3D('',#10085,#7985,#7986);
#6797=AXIS2_PLACEMENT_3D('',#10087,#7987,#7988);
#6798=AXIS2_PLACEMENT_3D('',#10088,#7989,#7990);
#6799=AXIS2_PLACEMENT_3D('',#10090,#7991,#7992);
#6800=AXIS2_PLACEMENT_3D('',#10092,#7994,#7995);
#6801=AXIS2_PLACEMENT_3D('',#10094,#7996,#7997);
#6802=AXIS2_PLACEMENT_3D('',#10097,#7999,#8000);
#6803=AXIS2_PLACEMENT_3D('',#10098,#8001,#8002);
#6804=AXIS2_PLACEMENT_3D('',#10099,#8003,#8004);
#6805=AXIS2_PLACEMENT_3D('',#10100,#8005,#8006);
#6806=AXIS2_PLACEMENT_3D('',#10101,#8007,#8008);
#6807=AXIS2_PLACEMENT_3D('',#10110,#8013,#8014);
#6808=AXIS2_PLACEMENT_3D('',#10116,#8018,#8019);
#6809=AXIS2_PLACEMENT_3D('',#10122,#8023,#8024);
#6810=AXIS2_PLACEMENT_3D('',#10128,#8028,#8029);
#6811=AXIS2_PLACEMENT_3D('',#10134,#8033,#8034);
#6812=AXIS2_PLACEMENT_3D('',#10137,#8037,#8038);
#6813=AXIS2_PLACEMENT_3D('',#10138,#8039,#8040);
#6814=AXIS2_PLACEMENT_3D('',#10139,#8041,#8042);
#6815=AXIS2_PLACEMENT_3D('',#10141,#8043,#8044);
#6816=AXIS2_PLACEMENT_3D('',#10142,#8045,#8046);
#6817=AXIS2_PLACEMENT_3D('',#10144,#8047,#8048);
#6818=AXIS2_PLACEMENT_3D('',#10145,#8049,#8050);
#6819=AXIS2_PLACEMENT_3D('',#10147,#8051,#8052);
#6820=AXIS2_PLACEMENT_3D('',#10149,#8054,#8055);
#6821=AXIS2_PLACEMENT_3D('',#10151,#8056,#8057);
#6822=AXIS2_PLACEMENT_3D('',#10153,#8059,#8060);
#6823=AXIS2_PLACEMENT_3D('',#10155,#8061,#8062);
#6824=AXIS2_PLACEMENT_3D('',#10157,#8064,#8065);
#6825=AXIS2_PLACEMENT_3D('',#10159,#8066,#8067);
#6826=AXIS2_PLACEMENT_3D('',#10160,#8068,#8069);
#6827=AXIS2_PLACEMENT_3D('',#10162,#8070,#8071);
#6828=AXIS2_PLACEMENT_3D('',#10164,#8073,#8074);
#6829=AXIS2_PLACEMENT_3D('',#10166,#8076,#8077);
#6830=AXIS2_PLACEMENT_3D('',#10167,#8078,#8079);
#6831=AXIS2_PLACEMENT_3D('',#10168,#8080,#8081);
#6832=AXIS2_PLACEMENT_3D('',#10171,#8082,#8083);
#6833=AXIS2_PLACEMENT_3D('',#10172,#8084,#8085);
#6834=AXIS2_PLACEMENT_3D('',#10174,#8086,#8087);
#6835=AXIS2_PLACEMENT_3D('',#10176,#8088,#8089);
#6836=AXIS2_PLACEMENT_3D('',#10177,#8090,#8091);
#6837=AXIS2_PLACEMENT_3D('',#10178,#8092,#8093);
#6838=AXIS2_PLACEMENT_3D('',#10181,#8095,#8096);
#6839=AXIS2_PLACEMENT_3D('',#10182,#8097,#8098);
#6840=AXIS2_PLACEMENT_3D('',#10184,#8099,#8100);
#6841=AXIS2_PLACEMENT_3D('',#10187,#8102,#8103);
#6842=AXIS2_PLACEMENT_3D('',#10188,#8104,#8105);
#6843=AXIS2_PLACEMENT_3D('',#10191,#8107,#8108);
#6844=AXIS2_PLACEMENT_3D('',#10192,#8109,#8110);
#6845=AXIS2_PLACEMENT_3D('',#10193,#8111,#8112);
#6846=AXIS2_PLACEMENT_3D('',#10195,#8113,#8114);
#6847=AXIS2_PLACEMENT_3D('',#10197,#8116,#8117);
#6848=AXIS2_PLACEMENT_3D('',#10199,#8118,#8119);
#6849=AXIS2_PLACEMENT_3D('',#10200,#8120,#8121);
#6850=AXIS2_PLACEMENT_3D('',#10202,#8123,#8124);
#6851=AXIS2_PLACEMENT_3D('',#10203,#8125,#8126);
#6852=AXIS2_PLACEMENT_3D('',#10206,#8127,#8128);
#6853=AXIS2_PLACEMENT_3D('',#10207,#8129,#8130);
#6854=AXIS2_PLACEMENT_3D('',#10209,#8131,#8132);
#6855=AXIS2_PLACEMENT_3D('',#10211,#8133,#8134);
#6856=AXIS2_PLACEMENT_3D('',#10212,#8135,#8136);
#6857=AXIS2_PLACEMENT_3D('',#10213,#8137,#8138);
#6858=AXIS2_PLACEMENT_3D('',#10215,#8139,#8140);
#6859=AXIS2_PLACEMENT_3D('',#10217,#8142,#8143);
#6860=AXIS2_PLACEMENT_3D('',#10219,#8144,#8145);
#6861=AXIS2_PLACEMENT_3D('',#10221,#8146,#8147);
#6862=AXIS2_PLACEMENT_3D('',#10222,#8148,#8149);
#6863=AXIS2_PLACEMENT_3D('',#10224,#8150,#8151);
#6864=AXIS2_PLACEMENT_3D('',#10226,#8153,#8154);
#6865=AXIS2_PLACEMENT_3D('',#10228,#8155,#8156);
#6866=AXIS2_PLACEMENT_3D('',#10230,#8158,#8159);
#6867=AXIS2_PLACEMENT_3D('',#10232,#8160,#8161);
#6868=AXIS2_PLACEMENT_3D('',#10234,#8163,#8164);
#6869=AXIS2_PLACEMENT_3D('',#10235,#8165,#8166);
#6870=AXIS2_PLACEMENT_3D('',#10237,#8168,#8169);
#6871=AXIS2_PLACEMENT_3D('',#10238,#8170,#8171);
#6872=AXIS2_PLACEMENT_3D('',#10241,#8172,#8173);
#6873=AXIS2_PLACEMENT_3D('',#10242,#8174,#8175);
#6874=AXIS2_PLACEMENT_3D('',#10245,#8176,#8177);
#6875=AXIS2_PLACEMENT_3D('',#10246,#8178,#8179);
#6876=AXIS2_PLACEMENT_3D('',#10249,#8180,#8181);
#6877=AXIS2_PLACEMENT_3D('',#10250,#8182,#8183);
#6878=AXIS2_PLACEMENT_3D('',#10253,#8184,#8185);
#6879=AXIS2_PLACEMENT_3D('',#10254,#8186,#8187);
#6880=AXIS2_PLACEMENT_3D('',#10257,#8188,#8189);
#6881=AXIS2_PLACEMENT_3D('',#10258,#8190,#8191);
#6882=AXIS2_PLACEMENT_3D('',#10261,#8192,#8193);
#6883=AXIS2_PLACEMENT_3D('',#10262,#8194,#8195);
#6884=AXIS2_PLACEMENT_3D('',#10265,#8196,#8197);
#6885=AXIS2_PLACEMENT_3D('',#10266,#8198,#8199);
#6886=AXIS2_PLACEMENT_3D('',#10269,#8200,#8201);
#6887=AXIS2_PLACEMENT_3D('',#10270,#8202,#8203);
#6888=AXIS2_PLACEMENT_3D('',#10271,#8204,#8205);
#6889=AXIS2_PLACEMENT_3D('',#10297,#8206,#8207);
#6890=AXIS2_PLACEMENT_3D('',#10321,#8208,#8209);
#6891=AXIS2_PLACEMENT_3D('',#10322,#8210,#8211);
#6892=AXIS2_PLACEMENT_3D('',#10324,#8212,#8213);
#6893=AXIS2_PLACEMENT_3D('',#10349,#8214,#8215);
#6894=AXIS2_PLACEMENT_3D('',#10374,#8216,#8217);
#6895=AXIS2_PLACEMENT_3D('',#10390,#8219,#8220);
#6896=AXIS2_PLACEMENT_3D('',#10405,#8221,#8222);
#6897=AXIS2_PLACEMENT_3D('',#10430,#8223,#8224);
#6898=AXIS2_PLACEMENT_3D('',#10455,#8225,#8226);
#6899=AXIS2_PLACEMENT_3D('',#10480,#8227,#8228);
#6900=AXIS2_PLACEMENT_3D('',#10504,#8229,#8230);
#6901=AXIS2_PLACEMENT_3D('',#10505,#8231,#8232);
#6902=AXIS2_PLACEMENT_3D('',#10507,#8233,#8234);
#6903=AXIS2_PLACEMENT_3D('',#10508,#8235,#8236);
#6904=AXIS2_PLACEMENT_3D('',#10509,#8237,#8238);
#6905=AXIS2_PLACEMENT_3D('',#10533,#8239,#8240);
#6906=AXIS2_PLACEMENT_3D('',#10534,#8241,#8242);
#6907=AXIS2_PLACEMENT_3D('',#10536,#8243,#8244);
#6908=AXIS2_PLACEMENT_3D('',#10537,#8245,#8246);
#6909=AXIS2_PLACEMENT_3D('',#10538,#8247,#8248);
#6910=AXIS2_PLACEMENT_3D('',#10562,#8249,#8250);
#6911=AXIS2_PLACEMENT_3D('',#10563,#8251,#8252);
#6912=AXIS2_PLACEMENT_3D('',#10565,#8253,#8254);
#6913=AXIS2_PLACEMENT_3D('',#10566,#8255,#8256);
#6914=AXIS2_PLACEMENT_3D('',#10567,#8257,#8258);
#6915=AXIS2_PLACEMENT_3D('',#10582,#8259,#8260);
#6916=AXIS2_PLACEMENT_3D('',#10595,#8261,#8262);
#6917=AXIS2_PLACEMENT_3D('',#10597,#8263,#8264);
#6918=AXIS2_PLACEMENT_3D('',#10598,#8265,#8266);
#6919=AXIS2_PLACEMENT_3D('',#10599,#8267,#8268);
#6920=AXIS2_PLACEMENT_3D('',#10623,#8269,#8270);
#6921=AXIS2_PLACEMENT_3D('',#10624,#8271,#8272);
#6922=AXIS2_PLACEMENT_3D('',#10626,#8273,#8274);
#6923=AXIS2_PLACEMENT_3D('',#10627,#8275,#8276);
#6924=AXIS2_PLACEMENT_3D('',#10628,#8277,#8278);
#6925=AXIS2_PLACEMENT_3D('',#10652,#8279,#8280);
#6926=AXIS2_PLACEMENT_3D('',#10653,#8281,#8282);
#6927=AXIS2_PLACEMENT_3D('',#10655,#8283,#8284);
#6928=AXIS2_PLACEMENT_3D('',#10656,#8285,#8286);
#6929=AXIS2_PLACEMENT_3D('',#10657,#8287,#8288);
#6930=AXIS2_PLACEMENT_3D('',#10681,#8289,#8290);
#6931=AXIS2_PLACEMENT_3D('',#10682,#8291,#8292);
#6932=AXIS2_PLACEMENT_3D('',#10684,#8293,#8294);
#6933=AXIS2_PLACEMENT_3D('',#10687,#8296,#8297);
#6934=AXIS2_PLACEMENT_3D('',#10711,#8298,#8299);
#6935=AXIS2_PLACEMENT_3D('',#10712,#8300,#8301);
#6936=AXIS2_PLACEMENT_3D('',#10713,#8302,#8303);
#6937=AXIS2_PLACEMENT_3D('',#10714,#8304,#8305);
#6938=AXIS2_PLACEMENT_3D('',#10715,#8306,#8307);
#6939=AXIS2_PLACEMENT_3D('',#10716,#8308,#8309);
#6940=AXIS2_PLACEMENT_3D('',#10717,#8310,#8311);
#6941=AXIS2_PLACEMENT_3D('',#10718,#8312,#8313);
#6942=AXIS2_PLACEMENT_3D('',#10719,#8314,#8315);
#6943=AXIS2_PLACEMENT_3D('',#10721,#8316,#8317);
#6944=AXIS2_PLACEMENT_3D('',#10723,#8318,#8319);
#6945=AXIS2_PLACEMENT_3D('',#10724,#8320,#8321);
#6946=AXIS2_PLACEMENT_3D('',#10726,#8322,#8323);
#6947=AXIS2_PLACEMENT_3D('',#10728,#8325,#8326);
#6948=AXIS2_PLACEMENT_3D('',#10730,#8327,#8328);
#6949=AXIS2_PLACEMENT_3D('',#10731,#8329,#8330);
#6950=AXIS2_PLACEMENT_3D('',#10733,#8332,#8333);
#6951=AXIS2_PLACEMENT_3D('',#10735,#8334,#8335);
#6952=AXIS2_PLACEMENT_3D('',#10737,#8336,#8337);
#6953=AXIS2_PLACEMENT_3D('',#10738,#8338,#8339);
#6954=AXIS2_PLACEMENT_3D('',#10740,#8340,#8341);
#6955=AXIS2_PLACEMENT_3D('',#10742,#8343,#8344);
#6956=AXIS2_PLACEMENT_3D('',#10744,#8345,#8346);
#6957=AXIS2_PLACEMENT_3D('',#10745,#8347,#8348);
#6958=AXIS2_PLACEMENT_3D('',#10747,#8350,#8351);
#6959=AXIS2_PLACEMENT_3D('',#10748,#8352,#8353);
#6960=AXIS2_PLACEMENT_3D('',#10749,#8354,#8355);
#6961=AXIS2_PLACEMENT_3D('',#10750,#8356,#8357);
#6962=AXIS2_PLACEMENT_3D('',#10751,#8358,#8359);
#6963=AXIS2_PLACEMENT_3D('',#10752,#8360,#8361);
#6964=AXIS2_PLACEMENT_3D('',#10753,#8362,#8363);
#6965=AXIS2_PLACEMENT_3D('',#10754,#8364,#8365);
#6966=AXIS2_PLACEMENT_3D('',#10756,#8366,#8367);
#6967=AXIS2_PLACEMENT_3D('',#10759,#8369,#8370);
#6968=AXIS2_PLACEMENT_3D('',#10760,#8371,#8372);
#6969=AXIS2_PLACEMENT_3D('',#10761,#8373,#8374);
#6970=AXIS2_PLACEMENT_3D('',#10763,#8375,#8376);
#6971=AXIS2_PLACEMENT_3D('',#10766,#8378,#8379);
#6972=AXIS2_PLACEMENT_3D('',#10767,#8380,#8381);
#6973=AXIS2_PLACEMENT_3D('',#10772,#8383,#8384);
#6974=AXIS2_PLACEMENT_3D('',#10775,#8386,#8387);
#6975=AXIS2_PLACEMENT_3D('',#10776,#8388,#8389);
#6976=AXIS2_PLACEMENT_3D('',#10782,#8393,#8394);
#6977=AXIS2_PLACEMENT_3D('',#10785,#8396,#8397);
#6978=AXIS2_PLACEMENT_3D('',#10787,#8398,#8399);
#6979=AXIS2_PLACEMENT_3D('',#10788,#8400,#8401);
#6980=AXIS2_PLACEMENT_3D('',#10792,#8404,#8405);
#6981=AXIS2_PLACEMENT_3D('',#10793,#8406,#8407);
#6982=AXIS2_PLACEMENT_3D('',#10794,#8408,#8409);
#6983=AXIS2_PLACEMENT_3D('',#10796,#8410,#8411);
#6984=AXIS2_PLACEMENT_3D('',#10797,#8412,#8413);
#6985=AXIS2_PLACEMENT_3D('',#10799,#8414,#8415);
#6986=AXIS2_PLACEMENT_3D('',#10801,#8416,#8417);
#6987=AXIS2_PLACEMENT_3D('',#10802,#8418,#8419);
#6988=AXIS2_PLACEMENT_3D('',#10804,#8421,#8422);
#6989=AXIS2_PLACEMENT_3D('',#10807,#8424,#8425);
#6990=AXIS2_PLACEMENT_3D('',#10808,#8426,#8427);
#6991=AXIS2_PLACEMENT_3D('',#10810,#8428,#8429);
#6992=AXIS2_PLACEMENT_3D('',#10812,#8431,#8432);
#6993=AXIS2_PLACEMENT_3D('',#10813,#8433,#8434);
#6994=AXIS2_PLACEMENT_3D('',#10814,#8435,#8436);
#6995=AXIS2_PLACEMENT_3D('',#10815,#8437,#8438);
#6996=AXIS2_PLACEMENT_3D('',#10817,#8439,#8440);
#6997=AXIS2_PLACEMENT_3D('',#10820,#8442,#8443);
#6998=AXIS2_PLACEMENT_3D('',#10821,#8444,#8445);
#6999=AXIS2_PLACEMENT_3D('',#10823,#8446,#8447);
#7000=AXIS2_PLACEMENT_3D('',#10826,#8449,#8450);
#7001=AXIS2_PLACEMENT_3D('',#10827,#8451,#8452);
#7002=AXIS2_PLACEMENT_3D('',#10828,#8453,#8454);
#7003=AXIS2_PLACEMENT_3D('',#10829,#8455,#8456);
#7004=AXIS2_PLACEMENT_3D('',#10830,#8457,#8458);
#7005=AXIS2_PLACEMENT_3D('',#10832,#8459,#8460);
#7006=AXIS2_PLACEMENT_3D('',#10835,#8462,#8463);
#7007=AXIS2_PLACEMENT_3D('',#10836,#8464,#8465);
#7008=AXIS2_PLACEMENT_3D('',#10838,#8466,#8467);
#7009=AXIS2_PLACEMENT_3D('',#10841,#8469,#8470);
#7010=AXIS2_PLACEMENT_3D('',#10842,#8471,#8472);
#7011=AXIS2_PLACEMENT_3D('',#10843,#8473,#8474);
#7012=AXIS2_PLACEMENT_3D('',#10844,#8475,#8476);
#7013=AXIS2_PLACEMENT_3D('',#10845,#8477,#8478);
#7014=AXIS2_PLACEMENT_3D('',#10849,#8480,#8481);
#7015=AXIS2_PLACEMENT_3D('',#10850,#8482,#8483);
#7016=AXIS2_PLACEMENT_3D('',#10867,#8484,#8485);
#7017=AXIS2_PLACEMENT_3D('',#10924,#8487,#8488);
#7018=AXIS2_PLACEMENT_3D('',#10926,#8490,#8491);
#7019=AXIS2_PLACEMENT_3D('',#10928,#8492,#8493);
#7020=AXIS2_PLACEMENT_3D('',#10931,#8495,#8496);
#7021=AXIS2_PLACEMENT_3D('',#10932,#8497,#8498);
#7022=AXIS2_PLACEMENT_3D('',#10934,#8499,#8500);
#7023=AXIS2_PLACEMENT_3D('',#10937,#8502,#8503);
#7024=AXIS2_PLACEMENT_3D('',#10938,#8504,#8505);
#7025=AXIS2_PLACEMENT_3D('',#10939,#8506,#8507);
#7026=AXIS2_PLACEMENT_3D('',#10940,#8508,#8509);
#7027=AXIS2_PLACEMENT_3D('',#10941,#8510,#8511);
#7028=AXIS2_PLACEMENT_3D('',#10945,#8513,#8514);
#7029=AXIS2_PLACEMENT_3D('',#10946,#8515,#8516);
#7030=AXIS2_PLACEMENT_3D('',#10959,#8517,#8518);
#7031=AXIS2_PLACEMENT_3D('',#11012,#8520,#8521);
#7032=AXIS2_PLACEMENT_3D('',#11014,#8523,#8524);
#7033=AXIS2_PLACEMENT_3D('',#11016,#8525,#8526);
#7034=AXIS2_PLACEMENT_3D('',#11019,#8528,#8529);
#7035=AXIS2_PLACEMENT_3D('',#11020,#8530,#8531);
#7036=AXIS2_PLACEMENT_3D('',#11022,#8532,#8533);
#7037=AXIS2_PLACEMENT_3D('',#11025,#8535,#8536);
#7038=AXIS2_PLACEMENT_3D('',#11026,#8537,#8538);
#7039=AXIS2_PLACEMENT_3D('',#11027,#8539,#8540);
#7040=AXIS2_PLACEMENT_3D('',#11028,#8541,#8542);
#7041=AXIS2_PLACEMENT_3D('',#11029,#8543,#8544);
#7042=AXIS2_PLACEMENT_3D('',#11031,#8545,#8546);
#7043=AXIS2_PLACEMENT_3D('',#11034,#8548,#8549);
#7044=AXIS2_PLACEMENT_3D('',#11035,#8550,#8551);
#7045=AXIS2_PLACEMENT_3D('',#11037,#8552,#8553);
#7046=AXIS2_PLACEMENT_3D('',#11040,#8555,#8556);
#7047=AXIS2_PLACEMENT_3D('',#11041,#8557,#8558);
#7048=AXIS2_PLACEMENT_3D('',#11042,#8559,#8560);
#7049=AXIS2_PLACEMENT_3D('',#11043,#8561,#8562);
#7050=AXIS2_PLACEMENT_3D('',#11044,#8563,#8564);
#7051=AXIS2_PLACEMENT_3D('',#11046,#8565,#8566);
#7052=AXIS2_PLACEMENT_3D('',#11049,#8568,#8569);
#7053=AXIS2_PLACEMENT_3D('',#11050,#8570,#8571);
#7054=AXIS2_PLACEMENT_3D('',#11051,#8572,#8573);
#7055=AXIS2_PLACEMENT_3D('',#11053,#8574,#8575);
#7056=AXIS2_PLACEMENT_3D('',#11056,#8577,#8578);
#7057=AXIS2_PLACEMENT_3D('',#11057,#8579,#8580);
#7058=AXIS2_PLACEMENT_3D('',#11058,#8581,#8582);
#7059=AXIS2_PLACEMENT_3D('',#11060,#8583,#8584);
#7060=AXIS2_PLACEMENT_3D('',#11062,#8585,#8586);
#7061=AXIS2_PLACEMENT_3D('',#11063,#8587,#8588);
#7062=AXIS2_PLACEMENT_3D('',#11065,#8589,#8590);
#7063=AXIS2_PLACEMENT_3D('',#11067,#8591,#8592);
#7064=AXIS2_PLACEMENT_3D('',#11068,#8593,#8594);
#7065=AXIS2_PLACEMENT_3D('',#11070,#8596,#8597);
#7066=AXIS2_PLACEMENT_3D('',#11073,#8599,#8600);
#7067=AXIS2_PLACEMENT_3D('',#11074,#8601,#8602);
#7068=AXIS2_PLACEMENT_3D('',#11076,#8603,#8604);
#7069=AXIS2_PLACEMENT_3D('',#11078,#8606,#8607);
#7070=AXIS2_PLACEMENT_3D('',#11079,#8608,#8609);
#7071=AXIS2_PLACEMENT_3D('',#11080,#8610,#8611);
#7072=AXIS2_PLACEMENT_3D('',#11081,#8612,#8613);
#7073=AXIS2_PLACEMENT_3D('',#11083,#8614,#8615);
#7074=AXIS2_PLACEMENT_3D('',#11086,#8617,#8618);
#7075=AXIS2_PLACEMENT_3D('',#11087,#8619,#8620);
#7076=AXIS2_PLACEMENT_3D('',#11089,#8621,#8622);
#7077=AXIS2_PLACEMENT_3D('',#11092,#8624,#8625);
#7078=AXIS2_PLACEMENT_3D('',#11093,#8626,#8627);
#7079=AXIS2_PLACEMENT_3D('',#11094,#8628,#8629);
#7080=AXIS2_PLACEMENT_3D('',#11095,#8630,#8631);
#7081=AXIS2_PLACEMENT_3D('',#11096,#8632,#8633);
#7082=AXIS2_PLACEMENT_3D('',#11098,#8634,#8635);
#7083=AXIS2_PLACEMENT_3D('',#11101,#8637,#8638);
#7084=AXIS2_PLACEMENT_3D('',#11102,#8639,#8640);
#7085=AXIS2_PLACEMENT_3D('',#11104,#8641,#8642);
#7086=AXIS2_PLACEMENT_3D('',#11107,#8644,#8645);
#7087=AXIS2_PLACEMENT_3D('',#11108,#8646,#8647);
#7088=AXIS2_PLACEMENT_3D('',#11109,#8648,#8649);
#7089=AXIS2_PLACEMENT_3D('',#11110,#8650,#8651);
#7090=AXIS2_PLACEMENT_3D('',#11111,#8652,#8653);
#7091=AXIS2_PLACEMENT_3D('',#11113,#8654,#8655);
#7092=AXIS2_PLACEMENT_3D('',#11116,#8657,#8658);
#7093=AXIS2_PLACEMENT_3D('',#11117,#8659,#8660);
#7094=AXIS2_PLACEMENT_3D('',#11119,#8661,#8662);
#7095=AXIS2_PLACEMENT_3D('',#11122,#8664,#8665);
#7096=AXIS2_PLACEMENT_3D('',#11123,#8666,#8667);
#7097=AXIS2_PLACEMENT_3D('',#11124,#8668,#8669);
#7098=AXIS2_PLACEMENT_3D('',#11125,#8670,#8671);
#7099=AXIS2_PLACEMENT_3D('',#11126,#8672,#8673);
#7100=AXIS2_PLACEMENT_3D('',#11128,#8674,#8675);
#7101=AXIS2_PLACEMENT_3D('',#11131,#8677,#8678);
#7102=AXIS2_PLACEMENT_3D('',#11132,#8679,#8680);
#7103=AXIS2_PLACEMENT_3D('',#11134,#8681,#8682);
#7104=AXIS2_PLACEMENT_3D('',#11137,#8684,#8685);
#7105=AXIS2_PLACEMENT_3D('',#11138,#8686,#8687);
#7106=AXIS2_PLACEMENT_3D('',#11139,#8688,#8689);
#7107=AXIS2_PLACEMENT_3D('',#11140,#8690,#8691);
#7108=AXIS2_PLACEMENT_3D('',#11141,#8692,#8693);
#7109=AXIS2_PLACEMENT_3D('',#11150,#8698,#8699);
#7110=AXIS2_PLACEMENT_3D('',#11156,#8703,#8704);
#7111=AXIS2_PLACEMENT_3D('',#11162,#8708,#8709);
#7112=AXIS2_PLACEMENT_3D('',#11168,#8713,#8714);
#7113=AXIS2_PLACEMENT_3D('',#11174,#8718,#8719);
#7114=AXIS2_PLACEMENT_3D('',#11177,#8722,#8723);
#7115=AXIS2_PLACEMENT_3D('',#11178,#8724,#8725);
#7116=AXIS2_PLACEMENT_3D('',#11180,#8726,#8727);
#7117=AXIS2_PLACEMENT_3D('',#11181,#8728,#8729);
#7118=AXIS2_PLACEMENT_3D('',#11183,#8730,#8731);
#7119=AXIS2_PLACEMENT_3D('',#11185,#8733,#8734);
#7120=AXIS2_PLACEMENT_3D('',#11187,#8735,#8736);
#7121=AXIS2_PLACEMENT_3D('',#11189,#8738,#8739);
#7122=AXIS2_PLACEMENT_3D('',#11191,#8740,#8741);
#7123=AXIS2_PLACEMENT_3D('',#11193,#8743,#8744);
#7124=AXIS2_PLACEMENT_3D('',#11194,#8745,#8746);
#7125=AXIS2_PLACEMENT_3D('',#11195,#8747,#8748);
#7126=AXIS2_PLACEMENT_3D('',#11196,#8749,#8750);
#7127=AXIS2_PLACEMENT_3D('',#11198,#8751,#8752);
#7128=AXIS2_PLACEMENT_3D('',#11201,#8754,#8755);
#7129=AXIS2_PLACEMENT_3D('',#11202,#8756,#8757);
#7130=AXIS2_PLACEMENT_3D('',#11204,#8758,#8759);
#7131=AXIS2_PLACEMENT_3D('',#11207,#8761,#8762);
#7132=AXIS2_PLACEMENT_3D('',#11208,#8763,#8764);
#7133=AXIS2_PLACEMENT_3D('',#11210,#8765,#8766);
#7134=AXIS2_PLACEMENT_3D('',#11213,#8768,#8769);
#7135=AXIS2_PLACEMENT_3D('',#11214,#8770,#8771);
#7136=AXIS2_PLACEMENT_3D('',#11216,#8772,#8773);
#7137=AXIS2_PLACEMENT_3D('',#11219,#8775,#8776);
#7138=AXIS2_PLACEMENT_3D('',#11220,#8777,#8778);
#7139=AXIS2_PLACEMENT_3D('',#11230,#8783,#8784);
#7140=AXIS2_PLACEMENT_3D('',#11231,#8785,#8786);
#7141=AXIS2_PLACEMENT_3D('',#11237,#8790,#8791);
#7142=AXIS2_PLACEMENT_3D('',#11241,#8794,#8795);
#7143=AXIS2_PLACEMENT_3D('',#11245,#8798,#8799);
#7144=AXIS2_PLACEMENT_3D('',#11247,#8801,#8802);
#7145=AXIS2_PLACEMENT_3D('',#11248,#8803,#8804);
#7146=AXIS2_PLACEMENT_3D('',#11251,#8806,#8807);
#7147=AXIS2_PLACEMENT_3D('',#11252,#8808,#8809);
#7148=AXIS2_PLACEMENT_3D('',#11254,#8810,#8811);
#7149=AXIS2_PLACEMENT_3D('',#11257,#8813,#8814);
#7150=AXIS2_PLACEMENT_3D('',#11258,#8815,#8816);
#7151=AXIS2_PLACEMENT_3D('',#11263,#8818,#8819);
#7152=AXIS2_PLACEMENT_3D('',#11266,#8821,#8822);
#7153=AXIS2_PLACEMENT_3D('',#11267,#8823,#8824);
#7154=AXIS2_PLACEMENT_3D('',#11273,#8828,#8829);
#7155=AXIS2_PLACEMENT_3D('',#11276,#8831,#8832);
#7156=AXIS2_PLACEMENT_3D('',#11277,#8833,#8834);
#7157=AXIS2_PLACEMENT_3D('',#11281,#8837,#8838);
#7158=AXIS2_PLACEMENT_3D('',#11282,#8839,#8840);
#7159=AXIS2_PLACEMENT_3D('',#11283,#8841,#8842);
#7160=AXIS2_PLACEMENT_3D('',#11285,#8843,#8844);
#7161=AXIS2_PLACEMENT_3D('',#11286,#8845,#8846);
#7162=AXIS2_PLACEMENT_3D('',#11288,#8847,#8848);
#7163=AXIS2_PLACEMENT_3D('',#11290,#8849,#8850);
#7164=AXIS2_PLACEMENT_3D('',#11291,#8851,#8852);
#7165=AXIS2_PLACEMENT_3D('',#11293,#8854,#8855);
#7166=AXIS2_PLACEMENT_3D('',#11296,#8857,#8858);
#7167=AXIS2_PLACEMENT_3D('',#11297,#8859,#8860);
#7168=AXIS2_PLACEMENT_3D('',#11298,#8861,#8862);
#7169=AXIS2_PLACEMENT_3D('',#11299,#8863,#8864);
#7170=AXIS2_PLACEMENT_3D('',#11301,#8865,#8866);
#7171=AXIS2_PLACEMENT_3D('',#11304,#8868,#8869);
#7172=AXIS2_PLACEMENT_3D('',#11305,#8870,#8871);
#7173=AXIS2_PLACEMENT_3D('',#11307,#8872,#8873);
#7174=AXIS2_PLACEMENT_3D('',#11310,#8875,#8876);
#7175=AXIS2_PLACEMENT_3D('',#11311,#8877,#8878);
#7176=AXIS2_PLACEMENT_3D('',#11312,#8879,#8880);
#7177=AXIS2_PLACEMENT_3D('',#11313,#8881,#8882);
#7178=AXIS2_PLACEMENT_3D('',#11314,#8883,#8884);
#7179=AXIS2_PLACEMENT_3D('',#11318,#8886,#8887);
#7180=AXIS2_PLACEMENT_3D('',#11319,#8888,#8889);
#7181=AXIS2_PLACEMENT_3D('',#11336,#8890,#8891);
#7182=AXIS2_PLACEMENT_3D('',#11393,#8893,#8894);
#7183=AXIS2_PLACEMENT_3D('',#11395,#8896,#8897);
#7184=AXIS2_PLACEMENT_3D('',#11397,#8898,#8899);
#7185=AXIS2_PLACEMENT_3D('',#11400,#8901,#8902);
#7186=AXIS2_PLACEMENT_3D('',#11401,#8903,#8904);
#7187=AXIS2_PLACEMENT_3D('',#11403,#8905,#8906);
#7188=AXIS2_PLACEMENT_3D('',#11406,#8908,#8909);
#7189=AXIS2_PLACEMENT_3D('',#11407,#8910,#8911);
#7190=AXIS2_PLACEMENT_3D('',#11408,#8912,#8913);
#7191=AXIS2_PLACEMENT_3D('',#11409,#8914,#8915);
#7192=AXIS2_PLACEMENT_3D('',#11410,#8916,#8917);
#7193=AXIS2_PLACEMENT_3D('',#11412,#8918,#8919);
#7194=AXIS2_PLACEMENT_3D('',#11415,#8921,#8922);
#7195=AXIS2_PLACEMENT_3D('',#11416,#8923,#8924);
#7196=AXIS2_PLACEMENT_3D('',#11417,#8925,#8926);
#7197=AXIS2_PLACEMENT_3D('',#11419,#8927,#8928);
#7198=AXIS2_PLACEMENT_3D('',#11422,#8930,#8931);
#7199=AXIS2_PLACEMENT_3D('',#11423,#8932,#8933);
#7200=AXIS2_PLACEMENT_3D('',#11424,#8934,#8935);
#7201=AXIS2_PLACEMENT_3D('',#11426,#8936,#8937);
#7202=AXIS2_PLACEMENT_3D('',#11428,#8938,#8939);
#7203=AXIS2_PLACEMENT_3D('',#11429,#8940,#8941);
#7204=AXIS2_PLACEMENT_3D('',#11431,#8942,#8943);
#7205=AXIS2_PLACEMENT_3D('',#11433,#8944,#8945);
#7206=AXIS2_PLACEMENT_3D('',#11434,#8946,#8947);
#7207=AXIS2_PLACEMENT_3D('',#11436,#8949,#8950);
#7208=AXIS2_PLACEMENT_3D('',#11439,#8952,#8953);
#7209=AXIS2_PLACEMENT_3D('',#11440,#8954,#8955);
#7210=AXIS2_PLACEMENT_3D('',#11442,#8956,#8957);
#7211=AXIS2_PLACEMENT_3D('',#11444,#8959,#8960);
#7212=AXIS2_PLACEMENT_3D('',#11445,#8961,#8962);
#7213=AXIS2_PLACEMENT_3D('',#11446,#8963,#8964);
#7214=AXIS2_PLACEMENT_3D('',#11447,#8965,#8966);
#7215=AXIS2_PLACEMENT_3D('',#11449,#8967,#8968);
#7216=AXIS2_PLACEMENT_3D('',#11452,#8970,#8971);
#7217=AXIS2_PLACEMENT_3D('',#11453,#8972,#8973);
#7218=AXIS2_PLACEMENT_3D('',#11455,#8974,#8975);
#7219=AXIS2_PLACEMENT_3D('',#11458,#8977,#8978);
#7220=AXIS2_PLACEMENT_3D('',#11459,#8979,#8980);
#7221=AXIS2_PLACEMENT_3D('',#11460,#8981,#8982);
#7222=AXIS2_PLACEMENT_3D('',#11461,#8983,#8984);
#7223=AXIS2_PLACEMENT_3D('',#11462,#8985,#8986);
#7224=AXIS2_PLACEMENT_3D('',#11464,#8987,#8988);
#7225=AXIS2_PLACEMENT_3D('',#11467,#8990,#8991);
#7226=AXIS2_PLACEMENT_3D('',#11468,#8992,#8993);
#7227=AXIS2_PLACEMENT_3D('',#11470,#8994,#8995);
#7228=AXIS2_PLACEMENT_3D('',#11473,#8997,#8998);
#7229=AXIS2_PLACEMENT_3D('',#11474,#8999,#9000);
#7230=AXIS2_PLACEMENT_3D('',#11475,#9001,#9002);
#7231=AXIS2_PLACEMENT_3D('',#11476,#9003,#9004);
#7232=AXIS2_PLACEMENT_3D('',#11477,#9005,#9006);
#7233=AXIS2_PLACEMENT_3D('',#11479,#9007,#9008);
#7234=AXIS2_PLACEMENT_3D('',#11482,#9010,#9011);
#7235=AXIS2_PLACEMENT_3D('',#11483,#9012,#9013);
#7236=AXIS2_PLACEMENT_3D('',#11485,#9014,#9015);
#7237=AXIS2_PLACEMENT_3D('',#11488,#9017,#9018);
#7238=AXIS2_PLACEMENT_3D('',#11489,#9019,#9020);
#7239=AXIS2_PLACEMENT_3D('',#11490,#9021,#9022);
#7240=AXIS2_PLACEMENT_3D('',#11491,#9023,#9024);
#7241=AXIS2_PLACEMENT_3D('',#11492,#9025,#9026);
#7242=AXIS2_PLACEMENT_3D('',#11494,#9027,#9028);
#7243=AXIS2_PLACEMENT_3D('',#11497,#9030,#9031);
#7244=AXIS2_PLACEMENT_3D('',#11498,#9032,#9033);
#7245=AXIS2_PLACEMENT_3D('',#11500,#9034,#9035);
#7246=AXIS2_PLACEMENT_3D('',#11503,#9037,#9038);
#7247=AXIS2_PLACEMENT_3D('',#11504,#9039,#9040);
#7248=AXIS2_PLACEMENT_3D('',#11505,#9041,#9042);
#7249=AXIS2_PLACEMENT_3D('',#11506,#9043,#9044);
#7250=AXIS2_PLACEMENT_3D('',#11507,#9045,#9046);
#7251=AXIS2_PLACEMENT_3D('',#11509,#9047,#9048);
#7252=AXIS2_PLACEMENT_3D('',#11510,#9049,#9050);
#7253=AXIS2_PLACEMENT_3D('',#11519,#9055,#9056);
#7254=AXIS2_PLACEMENT_3D('',#11525,#9060,#9061);
#7255=AXIS2_PLACEMENT_3D('',#11531,#9065,#9066);
#7256=AXIS2_PLACEMENT_3D('',#11537,#9070,#9071);
#7257=AXIS2_PLACEMENT_3D('',#11543,#9075,#9076);
#7258=AXIS2_PLACEMENT_3D('',#11546,#9079,#9080);
#7259=AXIS2_PLACEMENT_3D('',#11547,#9081,#9082);
#7260=AXIS2_PLACEMENT_3D('',#11549,#9083,#9084);
#7261=AXIS2_PLACEMENT_3D('',#11550,#9085,#9086);
#7262=AXIS2_PLACEMENT_3D('',#11552,#9087,#9088);
#7263=AXIS2_PLACEMENT_3D('',#11554,#9090,#9091);
#7264=AXIS2_PLACEMENT_3D('',#11556,#9093,#9094);
#7265=AXIS2_PLACEMENT_3D('',#11557,#9095,#9096);
#7266=AXIS2_PLACEMENT_3D('',#11559,#9097,#9098);
#7267=AXIS2_PLACEMENT_3D('',#11560,#9099,#9100);
#7268=AXIS2_PLACEMENT_3D('',#11562,#9101,#9102);
#7269=AXIS2_PLACEMENT_3D('',#11564,#9104,#9105);
#7270=AXIS2_PLACEMENT_3D('',#11566,#9106,#9107);
#7271=AXIS2_PLACEMENT_3D('',#11568,#9109,#9110);
#7272=AXIS2_PLACEMENT_3D('',#11570,#9111,#9112);
#7273=AXIS2_PLACEMENT_3D('',#11572,#9114,#9115);
#7274=AXIS2_PLACEMENT_3D('',#11574,#9116,#9117);
#7275=AXIS2_PLACEMENT_3D('',#11575,#9118,#9119);
#7276=AXIS2_PLACEMENT_3D('',#11577,#9120,#9121);
#7277=AXIS2_PLACEMENT_3D('',#11579,#9123,#9124);
#7278=AXIS2_PLACEMENT_3D('',#11581,#9125,#9126);
#7279=AXIS2_PLACEMENT_3D('',#11583,#9128,#9129);
#7280=AXIS2_PLACEMENT_3D('',#11585,#9130,#9131);
#7281=AXIS2_PLACEMENT_3D('',#11587,#9133,#9134);
#7282=AXIS2_PLACEMENT_3D('',#11588,#9135,#9136);
#7283=AXIS2_PLACEMENT_3D('',#11597,#9141,#9142);
#7284=AXIS2_PLACEMENT_3D('',#11603,#9146,#9147);
#7285=AXIS2_PLACEMENT_3D('',#11609,#9151,#9152);
#7286=AXIS2_PLACEMENT_3D('',#11615,#9156,#9157);
#7287=AXIS2_PLACEMENT_3D('',#11621,#9161,#9162);
#7288=AXIS2_PLACEMENT_3D('',#11624,#9165,#9166);
#7289=AXIS2_PLACEMENT_3D('',#11625,#9167,#9168);
#7290=AXIS2_PLACEMENT_3D('',#11626,#9169,#9170);
#7291=AXIS2_PLACEMENT_3D('',#11627,#9171,#9172);
#7292=AXIS2_PLACEMENT_3D('',#11636,#9177,#9178);
#7293=AXIS2_PLACEMENT_3D('',#11642,#9182,#9183);
#7294=AXIS2_PLACEMENT_3D('',#11648,#9187,#9188);
#7295=AXIS2_PLACEMENT_3D('',#11654,#9192,#9193);
#7296=AXIS2_PLACEMENT_3D('',#11660,#9197,#9198);
#7297=AXIS2_PLACEMENT_3D('',#11663,#9201,#9202);
#7298=AXIS2_PLACEMENT_3D('',#11664,#9203,#9204);
#7299=AXIS2_PLACEMENT_3D('',#11665,#9205,#9206);
#7300=AXIS2_PLACEMENT_3D('',#11667,#9207,#9208);
#7301=AXIS2_PLACEMENT_3D('',#11668,#9209,#9210);
#7302=AXIS2_PLACEMENT_3D('',#11670,#9211,#9212);
#7303=AXIS2_PLACEMENT_3D('',#11671,#9213,#9214);
#7304=AXIS2_PLACEMENT_3D('',#11673,#9215,#9216);
#7305=AXIS2_PLACEMENT_3D('',#11675,#9218,#9219);
#7306=AXIS2_PLACEMENT_3D('',#11677,#9220,#9221);
#7307=AXIS2_PLACEMENT_3D('',#11679,#9223,#9224);
#7308=AXIS2_PLACEMENT_3D('',#11681,#9225,#9226);
#7309=AXIS2_PLACEMENT_3D('',#11683,#9228,#9229);
#7310=AXIS2_PLACEMENT_3D('',#11685,#9230,#9231);
#7311=AXIS2_PLACEMENT_3D('',#11686,#9232,#9233);
#7312=AXIS2_PLACEMENT_3D('',#11688,#9234,#9235);
#7313=AXIS2_PLACEMENT_3D('',#11690,#9237,#9238);
#7314=AXIS2_PLACEMENT_3D('',#11692,#9240,#9241);
#7315=AXIS2_PLACEMENT_3D('',#11693,#9242,#9243);
#7316=AXIS2_PLACEMENT_3D('',#11694,#9244,#9245);
#7317=AXIS2_PLACEMENT_3D('',#11695,#9246,#9247);
#7318=AXIS2_PLACEMENT_3D('',#11696,#9248,#9249);
#7319=AXIS2_PLACEMENT_3D('',#11697,#9250,#9251);
#7320=AXIS2_PLACEMENT_3D('',#11698,#9252,#9253);
#7321=AXIS2_PLACEMENT_3D('',#11699,#9254,#9255);
#7322=AXIS2_PLACEMENT_3D('',#11700,#9256,#9257);
#7323=AXIS2_PLACEMENT_3D('',#11701,#9258,#9259);
#7324=AXIS2_PLACEMENT_3D('',#11702,#9260,#9261);
#7325=AXIS2_PLACEMENT_3D('',#11703,#9262,#9263);
#7326=AXIS2_PLACEMENT_3D('',#11704,#9264,#9265);
#7327=AXIS2_PLACEMENT_3D('',#11705,#9266,#9267);
#7328=AXIS2_PLACEMENT_3D('',#11706,#9268,#9269);
#7329=AXIS2_PLACEMENT_3D('',#11707,#9270,#9271);
#7330=AXIS2_PLACEMENT_3D('',#11708,#9272,#9273);
#7331=AXIS2_PLACEMENT_3D('',#11709,#9274,#9275);
#7332=AXIS2_PLACEMENT_3D('',#11710,#9276,#9277);
#7333=AXIS2_PLACEMENT_3D('',#11711,#9278,#9279);
#7334=AXIS2_PLACEMENT_3D('',#11712,#9280,#9281);
#7335=AXIS2_PLACEMENT_3D('',#11713,#9282,#9283);
#7336=AXIS2_PLACEMENT_3D('',#11714,#9284,#9285);
#7337=AXIS2_PLACEMENT_3D('',#11715,#9286,#9287);
#7338=AXIS2_PLACEMENT_3D('',#11716,#9288,#9289);
#7339=AXIS2_PLACEMENT_3D('',#11717,#9290,#9291);
#7340=AXIS2_PLACEMENT_3D('',#11718,#9292,#9293);
#7341=AXIS2_PLACEMENT_3D('',#11719,#9294,#9295);
#7342=AXIS2_PLACEMENT_3D('',#11720,#9296,#9297);
#7343=AXIS2_PLACEMENT_3D('',#11721,#9298,#9299);
#7344=AXIS2_PLACEMENT_3D('',#11722,#9300,#9301);
#7345=AXIS2_PLACEMENT_3D('',#11723,#9302,#9303);
#7346=AXIS2_PLACEMENT_3D('',#11724,#9304,#9305);
#7347=AXIS2_PLACEMENT_3D('',#11725,#9306,#9307);
#7348=AXIS2_PLACEMENT_3D('',#11726,#9308,#9309);
#7349=AXIS2_PLACEMENT_3D('',#11727,#9310,#9311);
#7350=AXIS2_PLACEMENT_3D('',#11728,#9312,#9313);
#7351=AXIS2_PLACEMENT_3D('',#11729,#9314,#9315);
#7352=AXIS2_PLACEMENT_3D('',#11730,#9316,#9317);
#7353=AXIS2_PLACEMENT_3D('',#11731,#9318,#9319);
#7354=AXIS2_PLACEMENT_3D('',#11732,#9320,#9321);
#7355=AXIS2_PLACEMENT_3D('',#11733,#9322,#9323);
#7356=AXIS2_PLACEMENT_3D('',#11734,#9324,#9325);
#7357=AXIS2_PLACEMENT_3D('',#11735,#9326,#9327);
#7358=AXIS2_PLACEMENT_3D('',#11736,#9328,#9329);
#7359=AXIS2_PLACEMENT_3D('',#11737,#9330,#9331);
#7360=AXIS2_PLACEMENT_3D('',#11738,#9332,#9333);
#7361=AXIS2_PLACEMENT_3D('',#11739,#9334,#9335);
#7362=AXIS2_PLACEMENT_3D('',#11740,#9336,#9337);
#7363=AXIS2_PLACEMENT_3D('',#11741,#9338,#9339);
#7364=AXIS2_PLACEMENT_3D('',#11742,#9340,#9341);
#7365=AXIS2_PLACEMENT_3D('',#11743,#9342,#9343);
#7366=AXIS2_PLACEMENT_3D('',#11744,#9344,#9345);
#7367=AXIS2_PLACEMENT_3D('',#11745,#9346,#9347);
#7368=AXIS2_PLACEMENT_3D('',#11746,#9348,#9349);
#7369=AXIS2_PLACEMENT_3D('',#11747,#9350,#9351);
#7370=AXIS2_PLACEMENT_3D('',#11748,#9352,#9353);
#7371=AXIS2_PLACEMENT_3D('',#11750,#9354,#9355);
#7372=AXIS2_PLACEMENT_3D('',#11753,#9357,#9358);
#7373=AXIS2_PLACEMENT_3D('',#11754,#9359,#9360);
#7374=AXIS2_PLACEMENT_3D('',#11756,#9361,#9362);
#7375=AXIS2_PLACEMENT_3D('',#11759,#9364,#9365);
#7376=AXIS2_PLACEMENT_3D('',#11760,#9366,#9367);
#7377=AXIS2_PLACEMENT_3D('',#11765,#9369,#9370);
#7378=AXIS2_PLACEMENT_3D('',#11768,#9372,#9373);
#7379=AXIS2_PLACEMENT_3D('',#11769,#9374,#9375);
#7380=AXIS2_PLACEMENT_3D('',#11775,#9379,#9380);
#7381=AXIS2_PLACEMENT_3D('',#11778,#9382,#9383);
#7382=AXIS2_PLACEMENT_3D('',#11779,#9384,#9385);
#7383=AXIS2_PLACEMENT_3D('',#11783,#9388,#9389);
#7384=AXIS2_PLACEMENT_3D('',#11784,#9390,#9391);
#7385=AXIS2_PLACEMENT_3D('',#11785,#9392,#9393);
#7386=AXIS2_PLACEMENT_3D('',#11786,#9394,#9395);
#7387=AXIS2_PLACEMENT_3D('',#11787,#9396,#9397);
#7388=AXIS2_PLACEMENT_3D('',#11789,#9398,#9399);
#7389=AXIS2_PLACEMENT_3D('',#11792,#9401,#9402);
#7390=AXIS2_PLACEMENT_3D('',#11793,#9403,#9404);
#7391=AXIS2_PLACEMENT_3D('',#11795,#9405,#9406);
#7392=AXIS2_PLACEMENT_3D('',#11798,#9408,#9409);
#7393=AXIS2_PLACEMENT_3D('',#11799,#9410,#9411);
#7394=AXIS2_PLACEMENT_3D('',#11800,#9412,#9413);
#7395=AXIS2_PLACEMENT_3D('',#11801,#9414,#9415);
#7396=AXIS2_PLACEMENT_3D('',#11802,#9416,#9417);
#7397=AXIS2_PLACEMENT_3D('',#11804,#9418,#9419);
#7398=AXIS2_PLACEMENT_3D('',#11807,#9421,#9422);
#7399=AXIS2_PLACEMENT_3D('',#11808,#9423,#9424);
#7400=AXIS2_PLACEMENT_3D('',#11810,#9425,#9426);
#7401=AXIS2_PLACEMENT_3D('',#11813,#9428,#9429);
#7402=AXIS2_PLACEMENT_3D('',#11814,#9430,#9431);
#7403=AXIS2_PLACEMENT_3D('',#11815,#9432,#9433);
#7404=AXIS2_PLACEMENT_3D('',#11816,#9434,#9435);
#7405=AXIS2_PLACEMENT_3D('',#11817,#9436,#9437);
#7406=AXIS2_PLACEMENT_3D('',#11818,#9438,#9439);
#7407=AXIS2_PLACEMENT_3D('',#11819,#9440,#9441);
#7408=AXIS2_PLACEMENT_3D('',#11820,#9442,#9443);
#7409=AXIS2_PLACEMENT_3D('',#11821,#9444,#9445);
#7410=AXIS2_PLACEMENT_3D('',#11822,#9446,#9447);
#7411=DIRECTION('axis',(0.,0.,1.));
#7412=DIRECTION('refdir',(1.,0.,0.));
#7413=DIRECTION('axis',(0.,0.,1.));
#7414=DIRECTION('refdir',(1.,0.,0.));
#7415=DIRECTION('axis',(0.,0.,1.));
#7416=DIRECTION('refdir',(1.,0.,0.));
#7417=DIRECTION('center_axis',(0.,0.,1.));
#7418=DIRECTION('ref_axis',(1.,0.,0.));
#7419=DIRECTION('center_axis',(0.,0.,1.));
#7420=DIRECTION('ref_axis',(1.,0.,0.));
#7421=DIRECTION('',(0.,0.,1.));
#7422=DIRECTION('center_axis',(0.,0.,-1.));
#7423=DIRECTION('ref_axis',(1.,0.,0.));
#7424=DIRECTION('center_axis',(0.,0.,1.));
#7425=DIRECTION('ref_axis',(1.,0.,0.));
#7426=DIRECTION('center_axis',(0.,0.,1.));
#7427=DIRECTION('ref_axis',(1.,0.,0.));
#7428=DIRECTION('',(0.,0.,1.));
#7429=DIRECTION('center_axis',(0.,0.,-1.));
#7430=DIRECTION('ref_axis',(1.,0.,0.));
#7431=DIRECTION('center_axis',(0.,0.,1.));
#7432=DIRECTION('ref_axis',(1.,0.,0.));
#7433=DIRECTION('center_axis',(0.,0.,1.));
#7434=DIRECTION('ref_axis',(1.,0.,0.));
#7435=DIRECTION('',(0.,0.,1.));
#7436=DIRECTION('center_axis',(0.,0.,-1.));
#7437=DIRECTION('ref_axis',(1.,0.,0.));
#7438=DIRECTION('center_axis',(0.,0.,1.));
#7439=DIRECTION('ref_axis',(1.,0.,0.));
#7440=DIRECTION('center_axis',(0.,0.,1.));
#7441=DIRECTION('ref_axis',(1.,0.,0.));
#7442=DIRECTION('',(0.,0.,1.));
#7443=DIRECTION('center_axis',(0.,0.,-1.));
#7444=DIRECTION('ref_axis',(1.,0.,0.));
#7445=DIRECTION('center_axis',(0.,0.,1.));
#7446=DIRECTION('ref_axis',(1.,0.,0.));
#7447=DIRECTION('center_axis',(0.,0.,1.));
#7448=DIRECTION('ref_axis',(1.,0.,0.));
#7449=DIRECTION('',(0.,0.,1.));
#7450=DIRECTION('center_axis',(0.,0.,-1.));
#7451=DIRECTION('ref_axis',(1.,0.,0.));
#7452=DIRECTION('center_axis',(0.,0.,1.));
#7453=DIRECTION('ref_axis',(1.,0.,0.));
#7454=DIRECTION('center_axis',(0.,0.,1.));
#7455=DIRECTION('ref_axis',(1.,0.,0.));
#7456=DIRECTION('',(0.,0.,1.));
#7457=DIRECTION('center_axis',(0.,0.,-1.));
#7458=DIRECTION('ref_axis',(1.,0.,0.));
#7459=DIRECTION('center_axis',(0.,0.,1.));
#7460=DIRECTION('ref_axis',(1.,0.,0.));
#7461=DIRECTION('center_axis',(0.,0.,1.));
#7462=DIRECTION('ref_axis',(1.,0.,0.));
#7463=DIRECTION('',(0.,0.,1.));
#7464=DIRECTION('center_axis',(0.,0.,-1.));
#7465=DIRECTION('ref_axis',(1.,0.,0.));
#7466=DIRECTION('center_axis',(0.,0.,1.));
#7467=DIRECTION('ref_axis',(1.,0.,0.));
#7468=DIRECTION('center_axis',(0.,0.,1.));
#7469=DIRECTION('ref_axis',(1.,0.,0.));
#7470=DIRECTION('',(0.,0.,1.));
#7471=DIRECTION('center_axis',(0.,0.,-1.));
#7472=DIRECTION('ref_axis',(1.,0.,0.));
#7473=DIRECTION('center_axis',(0.,1.,0.));
#7474=DIRECTION('ref_axis',(-1.,0.,0.));
#7475=DIRECTION('',(-1.,0.,0.));
#7476=DIRECTION('',(0.,0.,1.));
#7477=DIRECTION('',(-1.,0.,0.));
#7478=DIRECTION('',(0.,0.,1.));
#7479=DIRECTION('center_axis',(1.,0.,0.));
#7480=DIRECTION('ref_axis',(0.,1.,0.));
#7481=DIRECTION('',(0.,1.,0.));
#7482=DIRECTION('',(0.,1.,0.));
#7483=DIRECTION('',(0.,0.,1.));
#7484=DIRECTION('center_axis',(0.,-1.,0.));
#7485=DIRECTION('ref_axis',(1.,0.,0.));
#7486=DIRECTION('',(1.,0.,0.));
#7487=DIRECTION('',(1.,0.,0.));
#7488=DIRECTION('',(0.,0.,1.));
#7489=DIRECTION('center_axis',(-1.,0.,0.));
#7490=DIRECTION('ref_axis',(0.,-1.,0.));
#7491=DIRECTION('',(0.,-1.,0.));
#7492=DIRECTION('',(0.,-1.,0.));
#7493=DIRECTION('center_axis',(0.,0.,1.));
#7494=DIRECTION('ref_axis',(1.,0.,0.));
#7495=DIRECTION('center_axis',(0.,0.,1.));
#7496=DIRECTION('ref_axis',(1.,0.,0.));
#7497=DIRECTION('axis',(0.,0.,1.));
#7498=DIRECTION('refdir',(1.,0.,0.));
#7499=DIRECTION('center_axis',(0.,1.,0.));
#7500=DIRECTION('ref_axis',(-1.,0.,0.));
#7501=DIRECTION('',(-1.,0.,0.));
#7502=DIRECTION('',(0.,0.,1.));
#7503=DIRECTION('',(-1.,0.,0.));
#7504=DIRECTION('',(0.,0.,1.));
#7505=DIRECTION('center_axis',(1.,0.,0.));
#7506=DIRECTION('ref_axis',(0.,1.,0.));
#7507=DIRECTION('',(0.,1.,0.));
#7508=DIRECTION('',(0.,1.,0.));
#7509=DIRECTION('',(0.,0.,1.));
#7510=DIRECTION('center_axis',(0.,-1.,0.));
#7511=DIRECTION('ref_axis',(1.,0.,0.));
#7512=DIRECTION('',(1.,0.,0.));
#7513=DIRECTION('',(1.,0.,0.));
#7514=DIRECTION('',(0.,0.,1.));
#7515=DIRECTION('center_axis',(-1.,0.,0.));
#7516=DIRECTION('ref_axis',(0.,-1.,0.));
#7517=DIRECTION('',(0.,-1.,0.));
#7518=DIRECTION('',(0.,-1.,0.));
#7519=DIRECTION('center_axis',(0.,0.,1.));
#7520=DIRECTION('ref_axis',(1.,0.,0.));
#7521=DIRECTION('center_axis',(0.,0.,1.));
#7522=DIRECTION('ref_axis',(1.,0.,0.));
#7523=DIRECTION('axis',(0.,0.,1.));
#7524=DIRECTION('refdir',(1.,0.,0.));
#7525=DIRECTION('center_axis',(0.,1.,0.));
#7526=DIRECTION('ref_axis',(-1.,0.,0.));
#7527=DIRECTION('',(-1.,0.,0.));
#7528=DIRECTION('',(0.,0.,1.));
#7529=DIRECTION('',(-1.,0.,0.));
#7530=DIRECTION('',(0.,0.,1.));
#7531=DIRECTION('center_axis',(1.,0.,0.));
#7532=DIRECTION('ref_axis',(0.,1.,0.));
#7533=DIRECTION('',(0.,1.,0.));
#7534=DIRECTION('',(0.,1.,0.));
#7535=DIRECTION('',(0.,0.,1.));
#7536=DIRECTION('center_axis',(0.,-1.,0.));
#7537=DIRECTION('ref_axis',(1.,0.,0.));
#7538=DIRECTION('',(1.,0.,0.));
#7539=DIRECTION('',(1.,0.,0.));
#7540=DIRECTION('',(0.,0.,1.));
#7541=DIRECTION('center_axis',(-1.,0.,0.));
#7542=DIRECTION('ref_axis',(0.,-1.,0.));
#7543=DIRECTION('',(0.,-1.,0.));
#7544=DIRECTION('',(0.,-1.,0.));
#7545=DIRECTION('center_axis',(0.,0.,1.));
#7546=DIRECTION('ref_axis',(1.,0.,0.));
#7547=DIRECTION('center_axis',(0.,0.,1.));
#7548=DIRECTION('ref_axis',(1.,0.,0.));
#7549=DIRECTION('axis',(0.,0.,1.));
#7550=DIRECTION('refdir',(1.,0.,0.));
#7551=DIRECTION('center_axis',(0.,0.,1.));
#7552=DIRECTION('ref_axis',(1.,0.,0.));
#7553=DIRECTION('center_axis',(0.,0.,1.));
#7554=DIRECTION('ref_axis',(1.,0.,0.));
#7555=DIRECTION('center_axis',(0.,0.,1.));
#7556=DIRECTION('ref_axis',(1.,0.,0.));
#7557=DIRECTION('center_axis',(0.,0.,1.));
#7558=DIRECTION('ref_axis',(1.,0.,0.));
#7559=DIRECTION('',(0.,0.,1.));
#7560=DIRECTION('center_axis',(0.,0.,1.));
#7561=DIRECTION('ref_axis',(1.,0.,0.));
#7562=DIRECTION('',(0.,0.,-1.));
#7563=DIRECTION('center_axis',(0.,0.,1.));
#7564=DIRECTION('ref_axis',(1.,0.,0.));
#7565=DIRECTION('',(0.,0.,-1.));
#7566=DIRECTION('center_axis',(0.,0.,1.));
#7567=DIRECTION('ref_axis',(1.,0.,0.));
#7568=DIRECTION('',(0.,0.,1.));
#7569=DIRECTION('center_axis',(0.,0.,1.));
#7570=DIRECTION('ref_axis',(1.,0.,0.));
#7571=DIRECTION('center_axis',(0.,0.,1.));
#7572=DIRECTION('ref_axis',(1.,0.,0.));
#7573=DIRECTION('center_axis',(0.,0.,1.));
#7574=DIRECTION('ref_axis',(1.,0.,0.));
#7575=DIRECTION('center_axis',(0.,0.,1.));
#7576=DIRECTION('ref_axis',(-0.707106781186548,-0.707106781186547,0.));
#7577=DIRECTION('',(0.,0.,-1.));
#7578=DIRECTION('center_axis',(0.,0.,1.));
#7579=DIRECTION('ref_axis',(1.,0.,0.));
#7580=DIRECTION('',(0.,0.,1.));
#7581=DIRECTION('center_axis',(0.,0.,1.));
#7582=DIRECTION('ref_axis',(1.,0.,0.));
#7583=DIRECTION('center_axis',(0.,0.,1.));
#7584=DIRECTION('ref_axis',(1.,0.,0.));
#7585=DIRECTION('center_axis',(0.,0.,1.));
#7586=DIRECTION('ref_axis',(1.,0.,0.));
#7587=DIRECTION('center_axis',(0.,0.,1.));
#7588=DIRECTION('ref_axis',(-0.707106781186547,0.707106781186548,0.));
#7589=DIRECTION('',(0.,0.,-1.));
#7590=DIRECTION('center_axis',(0.,0.,1.));
#7591=DIRECTION('ref_axis',(1.,0.,0.));
#7592=DIRECTION('',(0.,0.,1.));
#7593=DIRECTION('center_axis',(0.,0.,1.));
#7594=DIRECTION('ref_axis',(1.,0.,0.));
#7595=DIRECTION('center_axis',(0.,0.,1.));
#7596=DIRECTION('ref_axis',(1.,0.,0.));
#7597=DIRECTION('center_axis',(0.,0.,1.));
#7598=DIRECTION('ref_axis',(1.,0.,0.));
#7599=DIRECTION('center_axis',(0.,0.,1.));
#7600=DIRECTION('ref_axis',(1.,0.,0.));
#7601=DIRECTION('center_axis',(0.,0.,1.));
#7602=DIRECTION('ref_axis',(1.,0.,0.));
#7603=DIRECTION('',(0.,0.,-1.));
#7604=DIRECTION('center_axis',(0.,0.,1.));
#7605=DIRECTION('ref_axis',(1.,0.,0.));
#7606=DIRECTION('center_axis',(0.,0.,1.));
#7607=DIRECTION('ref_axis',(1.,0.,0.));
#7608=DIRECTION('center_axis',(0.,0.,1.));
#7609=DIRECTION('ref_axis',(1.,0.,0.));
#7610=DIRECTION('center_axis',(0.,0.,1.));
#7611=DIRECTION('ref_axis',(1.,0.,0.));
#7612=DIRECTION('center_axis',(0.,0.,1.));
#7613=DIRECTION('ref_axis',(1.,0.,0.));
#7614=DIRECTION('center_axis',(0.,0.,1.));
#7615=DIRECTION('ref_axis',(1.,0.,0.));
#7616=DIRECTION('center_axis',(0.,0.,1.));
#7617=DIRECTION('ref_axis',(1.,0.,0.));
#7618=DIRECTION('center_axis',(0.,0.,-1.));
#7619=DIRECTION('ref_axis',(1.,0.,0.));
#7620=DIRECTION('center_axis',(0.,0.,-1.));
#7621=DIRECTION('ref_axis',(1.,0.,0.));
#7622=DIRECTION('center_axis',(0.,0.,-1.));
#7623=DIRECTION('ref_axis',(1.,0.,0.));
#7624=DIRECTION('center_axis',(0.,0.,-1.));
#7625=DIRECTION('ref_axis',(1.,0.,0.));
#7626=DIRECTION('center_axis',(0.,0.,1.));
#7627=DIRECTION('ref_axis',(1.,0.,0.));
#7628=DIRECTION('center_axis',(0.,0.,1.));
#7629=DIRECTION('ref_axis',(1.,0.,0.));
#7630=DIRECTION('',(0.,0.,1.));
#7631=DIRECTION('center_axis',(0.,0.,-1.));
#7632=DIRECTION('ref_axis',(1.,0.,0.));
#7633=DIRECTION('center_axis',(0.,0.,1.));
#7634=DIRECTION('ref_axis',(1.,0.,0.));
#7635=DIRECTION('center_axis',(0.,0.,1.));
#7636=DIRECTION('ref_axis',(1.,0.,0.));
#7637=DIRECTION('center_axis',(0.,0.,1.));
#7638=DIRECTION('ref_axis',(1.,0.,0.));
#7639=DIRECTION('',(0.,0.,1.));
#7640=DIRECTION('center_axis',(0.,0.,-1.));
#7641=DIRECTION('ref_axis',(1.,0.,0.));
#7642=DIRECTION('center_axis',(0.,0.,1.));
#7643=DIRECTION('ref_axis',(1.,0.,0.));
#7644=DIRECTION('center_axis',(0.,0.,1.));
#7645=DIRECTION('ref_axis',(1.,0.,0.));
#7646=DIRECTION('center_axis',(0.,0.,1.));
#7647=DIRECTION('ref_axis',(1.,0.,0.));
#7648=DIRECTION('',(0.,0.,1.));
#7649=DIRECTION('center_axis',(0.,0.,-1.));
#7650=DIRECTION('ref_axis',(1.,0.,0.));
#7651=DIRECTION('center_axis',(0.,0.,1.));
#7652=DIRECTION('ref_axis',(1.,0.,0.));
#7653=DIRECTION('center_axis',(0.,0.,1.));
#7654=DIRECTION('ref_axis',(1.,0.,0.));
#7655=DIRECTION('center_axis',(0.,0.,1.));
#7656=DIRECTION('ref_axis',(1.,0.,0.));
#7657=DIRECTION('',(0.,0.,1.));
#7658=DIRECTION('center_axis',(0.,0.,-1.));
#7659=DIRECTION('ref_axis',(1.,0.,0.));
#7660=DIRECTION('center_axis',(0.,0.,1.));
#7661=DIRECTION('ref_axis',(1.,0.,0.));
#7662=DIRECTION('center_axis',(1.,0.,0.));
#7663=DIRECTION('ref_axis',(0.,0.,-1.));
#7664=DIRECTION('',(1.,0.,0.));
#7665=DIRECTION('center_axis',(0.,0.,1.));
#7666=DIRECTION('ref_axis',(1.,0.,0.));
#7667=DIRECTION('center_axis',(0.,0.,1.));
#7668=DIRECTION('ref_axis',(1.,0.,0.));
#7669=DIRECTION('',(0.,0.,1.));
#7670=DIRECTION('center_axis',(0.,0.,1.));
#7671=DIRECTION('ref_axis',(1.,0.,0.));
#7672=DIRECTION('center_axis',(0.,0.,1.));
#7673=DIRECTION('ref_axis',(1.,0.,0.));
#7674=DIRECTION('',(0.,0.,1.));
#7675=DIRECTION('center_axis',(0.,0.,1.));
#7676=DIRECTION('ref_axis',(1.,0.,0.));
#7677=DIRECTION('center_axis',(0.,0.,1.));
#7678=DIRECTION('ref_axis',(1.,0.,0.));
#7679=DIRECTION('',(0.,0.,1.));
#7680=DIRECTION('center_axis',(0.,0.,1.));
#7681=DIRECTION('ref_axis',(1.,0.,0.));
#7682=DIRECTION('center_axis',(0.,0.,1.));
#7683=DIRECTION('ref_axis',(1.,0.,0.));
#7684=DIRECTION('',(0.,0.,1.));
#7685=DIRECTION('center_axis',(0.,0.,1.));
#7686=DIRECTION('ref_axis',(1.,0.,0.));
#7687=DIRECTION('center_axis',(0.,0.,1.));
#7688=DIRECTION('ref_axis',(1.,0.,0.));
#7689=DIRECTION('',(0.,0.,1.));
#7690=DIRECTION('center_axis',(0.,0.,-1.));
#7691=DIRECTION('ref_axis',(1.,0.,0.));
#7692=DIRECTION('center_axis',(0.,0.,1.));
#7693=DIRECTION('ref_axis',(1.,0.,0.));
#7694=DIRECTION('center_axis',(0.,0.,1.));
#7695=DIRECTION('ref_axis',(1.,0.,0.));
#7696=DIRECTION('center_axis',(0.,0.,1.));
#7697=DIRECTION('ref_axis',(1.,0.,0.));
#7698=DIRECTION('',(0.,0.,-1.));
#7699=DIRECTION('center_axis',(0.,0.,1.));
#7700=DIRECTION('ref_axis',(1.,0.,0.));
#7701=DIRECTION('center_axis',(0.,0.,1.));
#7702=DIRECTION('ref_axis',(1.,0.,0.));
#7703=DIRECTION('',(0.,0.,-1.));
#7704=DIRECTION('center_axis',(0.,0.,-1.));
#7705=DIRECTION('ref_axis',(1.,0.,0.));
#7706=DIRECTION('center_axis',(0.,0.,1.));
#7707=DIRECTION('ref_axis',(1.,0.,0.));
#7708=DIRECTION('center_axis',(0.,0.,1.));
#7709=DIRECTION('ref_axis',(1.,0.,0.));
#7710=DIRECTION('axis',(0.,0.,1.));
#7711=DIRECTION('refdir',(1.,0.,0.));
#7712=DIRECTION('center_axis',(0.,0.,1.));
#7713=DIRECTION('ref_axis',(1.,0.,0.));
#7714=DIRECTION('center_axis',(0.,0.,-1.));
#7715=DIRECTION('ref_axis',(1.,0.,0.));
#7716=DIRECTION('',(0.,0.,-1.));
#7717=DIRECTION('center_axis',(0.,0.,-1.));
#7718=DIRECTION('ref_axis',(1.,0.,0.));
#7719=DIRECTION('center_axis',(0.,0.,1.));
#7720=DIRECTION('ref_axis',(1.,0.,0.));
#7721=DIRECTION('center_axis',(0.,0.,1.));
#7722=DIRECTION('ref_axis',(1.,0.,0.));
#7723=DIRECTION('',(0.,0.,-1.));
#7724=DIRECTION('center_axis',(0.,0.,1.));
#7725=DIRECTION('ref_axis',(1.,0.,0.));
#7726=DIRECTION('center_axis',(0.,0.,1.));
#7727=DIRECTION('ref_axis',(1.,0.,0.));
#7728=DIRECTION('center_axis',(0.,0.,1.));
#7729=DIRECTION('ref_axis',(1.,0.,0.));
#7730=DIRECTION('axis',(0.,0.,1.));
#7731=DIRECTION('refdir',(1.,0.,0.));
#7732=DIRECTION('center_axis',(0.,0.,1.));
#7733=DIRECTION('ref_axis',(1.,0.,0.));
#7734=DIRECTION('center_axis',(0.,0.,1.));
#7735=DIRECTION('ref_axis',(1.,0.,0.));
#7736=DIRECTION('',(0.,0.,1.));
#7737=DIRECTION('center_axis',(0.,0.,-1.));
#7738=DIRECTION('ref_axis',(1.,0.,0.));
#7739=DIRECTION('center_axis',(0.,0.,1.));
#7740=DIRECTION('ref_axis',(1.,0.,0.));
#7741=DIRECTION('center_axis',(0.,0.,1.));
#7742=DIRECTION('ref_axis',(1.,0.,0.));
#7743=DIRECTION('',(0.,0.,1.));
#7744=DIRECTION('center_axis',(0.,0.,-1.));
#7745=DIRECTION('ref_axis',(1.,0.,0.));
#7746=DIRECTION('center_axis',(0.,0.,1.));
#7747=DIRECTION('ref_axis',(1.,0.,0.));
#7748=DIRECTION('center_axis',(0.,0.,1.));
#7749=DIRECTION('ref_axis',(1.,0.,0.));
#7750=DIRECTION('',(0.,0.,1.));
#7751=DIRECTION('center_axis',(0.,0.,-1.));
#7752=DIRECTION('ref_axis',(1.,0.,0.));
#7753=DIRECTION('center_axis',(0.,0.,1.));
#7754=DIRECTION('ref_axis',(1.,0.,0.));
#7755=DIRECTION('center_axis',(0.,0.,1.));
#7756=DIRECTION('ref_axis',(1.,0.,0.));
#7757=DIRECTION('',(0.,0.,1.));
#7758=DIRECTION('center_axis',(0.,0.,-1.));
#7759=DIRECTION('ref_axis',(1.,0.,0.));
#7760=DIRECTION('center_axis',(0.,0.,1.));
#7761=DIRECTION('ref_axis',(1.,0.,0.));
#7762=DIRECTION('center_axis',(0.,0.,1.));
#7763=DIRECTION('ref_axis',(1.,0.,0.));
#7764=DIRECTION('',(0.,0.,-1.));
#7765=DIRECTION('center_axis',(0.,0.,1.));
#7766=DIRECTION('ref_axis',(1.,0.,0.));
#7767=DIRECTION('center_axis',(0.,0.,1.));
#7768=DIRECTION('ref_axis',(1.,0.,0.));
#7769=DIRECTION('center_axis',(0.,0.,-1.));
#7770=DIRECTION('ref_axis',(1.,0.,0.));
#7771=DIRECTION('center_axis',(0.,0.,1.));
#7772=DIRECTION('ref_axis',(1.,0.,0.));
#7773=DIRECTION('center_axis',(0.,0.,-1.));
#7774=DIRECTION('ref_axis',(1.,0.,0.));
#7775=DIRECTION('',(0.,0.,-1.));
#7776=DIRECTION('center_axis',(0.,0.,1.));
#7777=DIRECTION('ref_axis',(1.,0.,0.));
#7778=DIRECTION('center_axis',(0.,0.,1.));
#7779=DIRECTION('ref_axis',(1.,0.,0.));
#7780=DIRECTION('',(0.,0.,-1.));
#7781=DIRECTION('center_axis',(0.,0.,1.));
#7782=DIRECTION('ref_axis',(1.,0.,0.));
#7783=DIRECTION('center_axis',(0.,0.,1.));
#7784=DIRECTION('ref_axis',(1.,0.,0.));
#7785=DIRECTION('center_axis',(0.,0.,1.));
#7786=DIRECTION('ref_axis',(1.,0.,0.));
#7787=DIRECTION('axis',(0.,0.,1.));
#7788=DIRECTION('refdir',(1.,0.,0.));
#7789=DIRECTION('center_axis',(0.,0.,1.));
#7790=DIRECTION('ref_axis',(1.,0.,0.));
#7791=DIRECTION('center_axis',(0.,0.,1.));
#7792=DIRECTION('ref_axis',(1.,0.,0.));
#7793=DIRECTION('center_axis',(0.,0.,1.));
#7794=DIRECTION('ref_axis',(1.,0.,0.));
#7795=DIRECTION('center_axis',(0.,0.,1.));
#7796=DIRECTION('ref_axis',(1.,0.,0.));
#7797=DIRECTION('',(0.,0.,1.));
#7798=DIRECTION('center_axis',(0.,0.,1.));
#7799=DIRECTION('ref_axis',(1.,0.,0.));
#7800=DIRECTION('',(0.,0.,-1.));
#7801=DIRECTION('center_axis',(0.,0.,1.));
#7802=DIRECTION('ref_axis',(1.,0.,0.));
#7803=DIRECTION('',(0.,0.,-1.));
#7804=DIRECTION('center_axis',(0.,0.,1.));
#7805=DIRECTION('ref_axis',(1.,0.,0.));
#7806=DIRECTION('',(0.,0.,1.));
#7807=DIRECTION('center_axis',(0.,0.,1.));
#7808=DIRECTION('ref_axis',(1.,0.,0.));
#7809=DIRECTION('center_axis',(0.,0.,1.));
#7810=DIRECTION('ref_axis',(1.,0.,0.));
#7811=DIRECTION('center_axis',(0.,0.,1.));
#7812=DIRECTION('ref_axis',(1.,0.,0.));
#7813=DIRECTION('center_axis',(0.,0.,1.));
#7814=DIRECTION('ref_axis',(-0.707106781186546,-0.707106781186549,0.));
#7815=DIRECTION('',(0.,0.,-1.));
#7816=DIRECTION('center_axis',(0.,0.,1.));
#7817=DIRECTION('ref_axis',(1.,0.,0.));
#7818=DIRECTION('',(0.,0.,1.));
#7819=DIRECTION('center_axis',(0.,0.,1.));
#7820=DIRECTION('ref_axis',(1.,0.,0.));
#7821=DIRECTION('center_axis',(0.,0.,1.));
#7822=DIRECTION('ref_axis',(1.,0.,0.));
#7823=DIRECTION('center_axis',(0.,0.,1.));
#7824=DIRECTION('ref_axis',(1.,0.,0.));
#7825=DIRECTION('center_axis',(0.,0.,1.));
#7826=DIRECTION('ref_axis',(-0.707106781186547,0.707106781186548,0.));
#7827=DIRECTION('',(0.,0.,-1.));
#7828=DIRECTION('center_axis',(0.,0.,1.));
#7829=DIRECTION('ref_axis',(1.,0.,0.));
#7830=DIRECTION('',(0.,0.,1.));
#7831=DIRECTION('center_axis',(0.,0.,1.));
#7832=DIRECTION('ref_axis',(1.,0.,0.));
#7833=DIRECTION('center_axis',(0.,0.,1.));
#7834=DIRECTION('ref_axis',(1.,0.,0.));
#7835=DIRECTION('center_axis',(0.,0.,1.));
#7836=DIRECTION('ref_axis',(1.,0.,0.));
#7837=DIRECTION('center_axis',(0.,0.,1.));
#7838=DIRECTION('ref_axis',(1.,0.,0.));
#7839=DIRECTION('center_axis',(0.,0.,1.));
#7840=DIRECTION('ref_axis',(1.,0.,0.));
#7841=DIRECTION('',(0.,0.,-1.));
#7842=DIRECTION('center_axis',(0.,0.,1.));
#7843=DIRECTION('ref_axis',(1.,0.,0.));
#7844=DIRECTION('center_axis',(0.,0.,1.));
#7845=DIRECTION('ref_axis',(1.,0.,0.));
#7846=DIRECTION('center_axis',(0.,0.,1.));
#7847=DIRECTION('ref_axis',(1.,0.,0.));
#7848=DIRECTION('center_axis',(0.,0.,1.));
#7849=DIRECTION('ref_axis',(1.,0.,0.));
#7850=DIRECTION('center_axis',(0.,0.,1.));
#7851=DIRECTION('ref_axis',(1.,0.,0.));
#7852=DIRECTION('center_axis',(0.,0.,1.));
#7853=DIRECTION('ref_axis',(1.,0.,0.));
#7854=DIRECTION('center_axis',(0.,0.,1.));
#7855=DIRECTION('ref_axis',(1.,0.,0.));
#7856=DIRECTION('center_axis',(0.,0.,-1.));
#7857=DIRECTION('ref_axis',(1.,0.,0.));
#7858=DIRECTION('center_axis',(0.,0.,-1.));
#7859=DIRECTION('ref_axis',(1.,0.,0.));
#7860=DIRECTION('center_axis',(0.,0.,-1.));
#7861=DIRECTION('ref_axis',(1.,0.,0.));
#7862=DIRECTION('center_axis',(0.,0.,-1.));
#7863=DIRECTION('ref_axis',(1.,0.,0.));
#7864=DIRECTION('center_axis',(0.,0.,1.));
#7865=DIRECTION('ref_axis',(1.,0.,0.));
#7866=DIRECTION('center_axis',(0.,0.,1.));
#7867=DIRECTION('ref_axis',(1.,0.,0.));
#7868=DIRECTION('',(0.,0.,1.));
#7869=DIRECTION('center_axis',(0.,0.,-1.));
#7870=DIRECTION('ref_axis',(1.,0.,0.));
#7871=DIRECTION('center_axis',(0.,0.,1.));
#7872=DIRECTION('ref_axis',(1.,0.,0.));
#7873=DIRECTION('center_axis',(0.,0.,1.));
#7874=DIRECTION('ref_axis',(1.,0.,0.));
#7875=DIRECTION('center_axis',(0.,0.,1.));
#7876=DIRECTION('ref_axis',(1.,0.,0.));
#7877=DIRECTION('',(0.,0.,1.));
#7878=DIRECTION('center_axis',(0.,0.,-1.));
#7879=DIRECTION('ref_axis',(1.,0.,0.));
#7880=DIRECTION('center_axis',(0.,0.,1.));
#7881=DIRECTION('ref_axis',(1.,0.,0.));
#7882=DIRECTION('center_axis',(0.,0.,1.));
#7883=DIRECTION('ref_axis',(1.,0.,0.));
#7884=DIRECTION('center_axis',(0.,0.,1.));
#7885=DIRECTION('ref_axis',(1.,0.,0.));
#7886=DIRECTION('',(0.,0.,1.));
#7887=DIRECTION('center_axis',(0.,0.,-1.));
#7888=DIRECTION('ref_axis',(1.,0.,0.));
#7889=DIRECTION('center_axis',(0.,0.,1.));
#7890=DIRECTION('ref_axis',(1.,0.,0.));
#7891=DIRECTION('center_axis',(0.,0.,1.));
#7892=DIRECTION('ref_axis',(1.,0.,0.));
#7893=DIRECTION('center_axis',(0.,0.,1.));
#7894=DIRECTION('ref_axis',(1.,0.,0.));
#7895=DIRECTION('',(0.,0.,1.));
#7896=DIRECTION('center_axis',(0.,0.,-1.));
#7897=DIRECTION('ref_axis',(1.,0.,0.));
#7898=DIRECTION('center_axis',(0.,0.,1.));
#7899=DIRECTION('ref_axis',(1.,0.,0.));
#7900=DIRECTION('center_axis',(1.,0.,0.));
#7901=DIRECTION('ref_axis',(0.,0.,-1.));
#7902=DIRECTION('',(1.,0.,0.));
#7903=DIRECTION('center_axis',(0.,0.,1.));
#7904=DIRECTION('ref_axis',(1.,0.,0.));
#7905=DIRECTION('center_axis',(0.,0.,1.));
#7906=DIRECTION('ref_axis',(1.,0.,0.));
#7907=DIRECTION('',(0.,0.,1.));
#7908=DIRECTION('center_axis',(0.,0.,1.));
#7909=DIRECTION('ref_axis',(1.,0.,0.));
#7910=DIRECTION('center_axis',(0.,0.,1.));
#7911=DIRECTION('ref_axis',(1.,0.,0.));
#7912=DIRECTION('',(0.,0.,1.));
#7913=DIRECTION('center_axis',(0.,0.,1.));
#7914=DIRECTION('ref_axis',(1.,0.,0.));
#7915=DIRECTION('center_axis',(0.,0.,1.));
#7916=DIRECTION('ref_axis',(1.,0.,0.));
#7917=DIRECTION('',(0.,0.,1.));
#7918=DIRECTION('center_axis',(0.,0.,1.));
#7919=DIRECTION('ref_axis',(1.,0.,0.));
#7920=DIRECTION('center_axis',(0.,0.,1.));
#7921=DIRECTION('ref_axis',(1.,0.,0.));
#7922=DIRECTION('',(0.,0.,1.));
#7923=DIRECTION('center_axis',(0.,0.,1.));
#7924=DIRECTION('ref_axis',(1.,0.,0.));
#7925=DIRECTION('center_axis',(0.,0.,1.));
#7926=DIRECTION('ref_axis',(1.,0.,0.));
#7927=DIRECTION('',(0.,0.,1.));
#7928=DIRECTION('center_axis',(0.,0.,-1.));
#7929=DIRECTION('ref_axis',(1.,0.,0.));
#7930=DIRECTION('center_axis',(0.,0.,1.));
#7931=DIRECTION('ref_axis',(1.,0.,0.));
#7932=DIRECTION('center_axis',(0.,0.,1.));
#7933=DIRECTION('ref_axis',(1.,0.,0.));
#7934=DIRECTION('center_axis',(0.,0.,1.));
#7935=DIRECTION('ref_axis',(1.,0.,0.));
#7936=DIRECTION('',(0.,0.,-1.));
#7937=DIRECTION('center_axis',(0.,0.,1.));
#7938=DIRECTION('ref_axis',(1.,0.,0.));
#7939=DIRECTION('center_axis',(0.,0.,1.));
#7940=DIRECTION('ref_axis',(1.,0.,0.));
#7941=DIRECTION('',(0.,0.,-1.));
#7942=DIRECTION('center_axis',(0.,0.,-1.));
#7943=DIRECTION('ref_axis',(1.,0.,0.));
#7944=DIRECTION('center_axis',(0.,0.,1.));
#7945=DIRECTION('ref_axis',(1.,0.,0.));
#7946=DIRECTION('center_axis',(0.,0.,1.));
#7947=DIRECTION('ref_axis',(1.,0.,0.));
#7948=DIRECTION('axis',(0.,0.,1.));
#7949=DIRECTION('refdir',(1.,0.,0.));
#7950=DIRECTION('center_axis',(0.,0.,1.));
#7951=DIRECTION('ref_axis',(1.,0.,0.));
#7952=DIRECTION('center_axis',(0.,0.,1.));
#7953=DIRECTION('ref_axis',(1.,0.,0.));
#7954=DIRECTION('',(0.,0.,1.));
#7955=DIRECTION('center_axis',(0.,0.,-1.));
#7956=DIRECTION('ref_axis',(1.,0.,0.));
#7957=DIRECTION('center_axis',(0.,0.,1.));
#7958=DIRECTION('ref_axis',(1.,0.,0.));
#7959=DIRECTION('center_axis',(0.,0.,1.));
#7960=DIRECTION('ref_axis',(1.,0.,0.));
#7961=DIRECTION('',(0.,0.,1.));
#7962=DIRECTION('center_axis',(0.,0.,-1.));
#7963=DIRECTION('ref_axis',(1.,0.,0.));
#7964=DIRECTION('center_axis',(0.,0.,1.));
#7965=DIRECTION('ref_axis',(1.,0.,0.));
#7966=DIRECTION('center_axis',(0.,0.,1.));
#7967=DIRECTION('ref_axis',(1.,0.,0.));
#7968=DIRECTION('',(0.,0.,1.));
#7969=DIRECTION('center_axis',(0.,0.,-1.));
#7970=DIRECTION('ref_axis',(1.,0.,0.));
#7971=DIRECTION('center_axis',(0.,0.,1.));
#7972=DIRECTION('ref_axis',(1.,0.,0.));
#7973=DIRECTION('center_axis',(0.,0.,1.));
#7974=DIRECTION('ref_axis',(1.,0.,0.));
#7975=DIRECTION('',(0.,0.,1.));
#7976=DIRECTION('center_axis',(0.,0.,-1.));
#7977=DIRECTION('ref_axis',(1.,0.,0.));
#7978=DIRECTION('center_axis',(0.,0.,1.));
#7979=DIRECTION('ref_axis',(1.,0.,0.));
#7980=DIRECTION('center_axis',(0.,0.,1.));
#7981=DIRECTION('ref_axis',(1.,0.,0.));
#7982=DIRECTION('',(0.,0.,-1.));
#7983=DIRECTION('center_axis',(0.,0.,1.));
#7984=DIRECTION('ref_axis',(1.,0.,0.));
#7985=DIRECTION('center_axis',(0.,0.,1.));
#7986=DIRECTION('ref_axis',(1.,0.,0.));
#7987=DIRECTION('center_axis',(0.,0.,-1.));
#7988=DIRECTION('ref_axis',(1.,0.,0.));
#7989=DIRECTION('center_axis',(0.,0.,1.));
#7990=DIRECTION('ref_axis',(1.,0.,0.));
#7991=DIRECTION('center_axis',(0.,0.,-1.));
#7992=DIRECTION('ref_axis',(1.,0.,0.));
#7993=DIRECTION('',(0.,0.,-1.));
#7994=DIRECTION('center_axis',(0.,0.,1.));
#7995=DIRECTION('ref_axis',(1.,0.,0.));
#7996=DIRECTION('center_axis',(0.,0.,1.));
#7997=DIRECTION('ref_axis',(1.,0.,0.));
#7998=DIRECTION('',(0.,0.,-1.));
#7999=DIRECTION('center_axis',(0.,0.,1.));
#8000=DIRECTION('ref_axis',(1.,0.,0.));
#8001=DIRECTION('center_axis',(0.,0.,1.));
#8002=DIRECTION('ref_axis',(1.,0.,0.));
#8003=DIRECTION('center_axis',(0.,0.,1.));
#8004=DIRECTION('ref_axis',(1.,0.,0.));
#8005=DIRECTION('axis',(0.,0.,1.));
#8006=DIRECTION('refdir',(1.,0.,0.));
#8007=DIRECTION('center_axis',(0.866025403784439,0.,-0.5));
#8008=DIRECTION('ref_axis',(0.5,0.,0.866025403784439));
#8009=DIRECTION('',(-0.5,0.,-0.866025403784439));
#8010=DIRECTION('',(0.,-1.,0.));
#8011=DIRECTION('',(0.5,0.,0.866025403784439));
#8012=DIRECTION('',(0.,-1.,0.));
#8013=DIRECTION('center_axis',(1.20185167898973E-16,0.,-1.));
#8014=DIRECTION('ref_axis',(1.,0.,1.20185167898973E-16));
#8015=DIRECTION('',(-1.,0.,-1.20185167898973E-16));
#8016=DIRECTION('',(0.,-1.,0.));
#8017=DIRECTION('',(1.,0.,1.20185167898973E-16));
#8018=DIRECTION('center_axis',(-0.866025403784439,0.,-0.5));
#8019=DIRECTION('ref_axis',(0.5,0.,-0.866025403784439));
#8020=DIRECTION('',(-0.5,0.,0.866025403784439));
#8021=DIRECTION('',(0.,-1.,0.));
#8022=DIRECTION('',(0.5,0.,-0.866025403784439));
#8023=DIRECTION('center_axis',(-0.866025403784439,0.,0.5));
#8024=DIRECTION('ref_axis',(-0.5,0.,-0.866025403784439));
#8025=DIRECTION('',(0.5,0.,0.866025403784439));
#8026=DIRECTION('',(0.,-1.,0.));
#8027=DIRECTION('',(-0.5,0.,-0.866025403784439));
#8028=DIRECTION('center_axis',(-2.40370335797945E-16,0.,1.));
#8029=DIRECTION('ref_axis',(-1.,0.,-2.40370335797945E-16));
#8030=DIRECTION('',(1.,0.,2.40370335797945E-16));
#8031=DIRECTION('',(0.,-1.,0.));
#8032=DIRECTION('',(-1.,0.,-2.40370335797945E-16));
#8033=DIRECTION('center_axis',(0.866025403784439,0.,0.5));
#8034=DIRECTION('ref_axis',(-0.5,0.,0.866025403784439));
#8035=DIRECTION('',(0.5,0.,-0.866025403784439));
#8036=DIRECTION('',(-0.5,0.,0.866025403784439));
#8037=DIRECTION('center_axis',(0.,1.,0.));
#8038=DIRECTION('ref_axis',(1.,0.,0.));
#8039=DIRECTION('center_axis',(0.,-1.,0.));
#8040=DIRECTION('ref_axis',(0.,0.,-1.));
#8041=DIRECTION('center_axis',(0.,1.,0.));
#8042=DIRECTION('ref_axis',(1.,0.,0.));
#8043=DIRECTION('center_axis',(0.,1.,0.));
#8044=DIRECTION('ref_axis',(1.,0.,0.));
#8045=DIRECTION('center_axis',(0.,1.,0.));
#8046=DIRECTION('ref_axis',(0.,0.,1.));
#8047=DIRECTION('center_axis',(0.,-1.,0.));
#8048=DIRECTION('ref_axis',(1.,0.,0.));
#8049=DIRECTION('center_axis',(0.,-1.,0.));
#8050=DIRECTION('ref_axis',(1.,0.,0.));
#8051=DIRECTION('center_axis',(0.,-1.,0.));
#8052=DIRECTION('ref_axis',(1.,0.,0.));
#8053=DIRECTION('',(0.707106781186548,0.707106781186547,8.65956056235493E-17));
#8054=DIRECTION('center_axis',(0.,-1.,0.));
#8055=DIRECTION('ref_axis',(1.,0.,0.));
#8056=DIRECTION('center_axis',(0.,-1.,0.));
#8057=DIRECTION('ref_axis',(1.,0.,0.));
#8058=DIRECTION('',(0.,1.,0.));
#8059=DIRECTION('center_axis',(0.,1.,0.));
#8060=DIRECTION('ref_axis',(1.,0.,0.));
#8061=DIRECTION('center_axis',(0.,-1.,0.));
#8062=DIRECTION('ref_axis',(1.,0.,0.));
#8063=DIRECTION('',(-0.707106781186547,0.707106781186548,-8.65956056235493E-17));
#8064=DIRECTION('center_axis',(0.,-1.,0.));
#8065=DIRECTION('ref_axis',(0.,0.,-1.));
#8066=DIRECTION('center_axis',(0.,-1.,0.));
#8067=DIRECTION('ref_axis',(1.,0.,0.));
#8068=DIRECTION('center_axis',(0.,1.,0.));
#8069=DIRECTION('ref_axis',(1.,0.,0.));
#8070=DIRECTION('center_axis',(0.,1.,0.));
#8071=DIRECTION('ref_axis',(1.,0.,0.));
#8072=DIRECTION('',(-0.447213595499958,0.894427190999916,-5.47678698264203E-17));
#8073=DIRECTION('center_axis',(0.,-1.,0.));
#8074=DIRECTION('ref_axis',(1.,0.,0.));
#8075=DIRECTION('',(0.,1.,0.));
#8076=DIRECTION('axis',(0.,0.,1.));
#8077=DIRECTION('refdir',(1.,0.,0.));
#8078=DIRECTION('axis',(0.,0.,1.));
#8079=DIRECTION('refdir',(1.,0.,0.));
#8080=DIRECTION('center_axis',(0.,-1.,0.));
#8081=DIRECTION('ref_axis',(0.,0.,-1.));
#8082=DIRECTION('center_axis',(0.,-1.,0.));
#8083=DIRECTION('ref_axis',(1.,0.,0.));
#8084=DIRECTION('center_axis',(0.,-1.,0.));
#8085=DIRECTION('ref_axis',(1.,0.,0.));
#8086=DIRECTION('center_axis',(1.,0.,1.22464679914735E-16));
#8087=DIRECTION('ref_axis',(-1.22464679914735E-16,0.,1.));
#8088=DIRECTION('center_axis',(0.,1.,0.));
#8089=DIRECTION('ref_axis',(1.,0.,0.));
#8090=DIRECTION('center_axis',(0.,1.,0.));
#8091=DIRECTION('ref_axis',(1.,0.,0.));
#8092=DIRECTION('center_axis',(0.,-1.,0.));
#8093=DIRECTION('ref_axis',(1.,0.,0.));
#8094=DIRECTION('',(0.,1.,0.));
#8095=DIRECTION('center_axis',(0.,-1.,0.));
#8096=DIRECTION('ref_axis',(1.,0.,0.));
#8097=DIRECTION('center_axis',(0.,-1.,0.));
#8098=DIRECTION('ref_axis',(1.,0.,0.));
#8099=DIRECTION('center_axis',(0.,-1.,0.));
#8100=DIRECTION('ref_axis',(1.,0.,0.));
#8101=DIRECTION('',(0.,1.,0.));
#8102=DIRECTION('center_axis',(0.,-1.,0.));
#8103=DIRECTION('ref_axis',(1.,0.,0.));
#8104=DIRECTION('center_axis',(0.,1.,0.));
#8105=DIRECTION('ref_axis',(1.,0.,0.));
#8106=DIRECTION('',(-0.707106781186547,0.707106781186548,-8.65956056235493E-17));
#8107=DIRECTION('center_axis',(0.,-1.,0.));
#8108=DIRECTION('ref_axis',(1.,0.,0.));
#8109=DIRECTION('center_axis',(0.,1.,0.));
#8110=DIRECTION('ref_axis',(0.,0.,1.));
#8111=DIRECTION('center_axis',(0.,-1.,0.));
#8112=DIRECTION('ref_axis',(1.,0.,0.));
#8113=DIRECTION('center_axis',(0.,-1.,0.));
#8114=DIRECTION('ref_axis',(1.,0.,0.));
#8115=DIRECTION('',(0.,1.,0.));
#8116=DIRECTION('center_axis',(0.,-1.,0.));
#8117=DIRECTION('ref_axis',(0.,0.,-1.));
#8118=DIRECTION('center_axis',(0.,-1.,0.));
#8119=DIRECTION('ref_axis',(1.,0.,0.));
#8120=DIRECTION('center_axis',(0.,-1.,0.));
#8121=DIRECTION('ref_axis',(1.,0.,0.));
#8122=DIRECTION('',(0.707106781186547,0.707106781186548,8.65956056235493E-17));
#8123=DIRECTION('axis',(0.,0.,1.));
#8124=DIRECTION('refdir',(1.,0.,0.));
#8125=DIRECTION('center_axis',(0.,-1.,0.));
#8126=DIRECTION('ref_axis',(0.,0.,-1.));
#8127=DIRECTION('center_axis',(0.,-1.,0.));
#8128=DIRECTION('ref_axis',(1.,0.,0.));
#8129=DIRECTION('center_axis',(0.,-1.,0.));
#8130=DIRECTION('ref_axis',(1.,0.,0.));
#8131=DIRECTION('center_axis',(1.,0.,1.22464679914735E-16));
#8132=DIRECTION('ref_axis',(-1.22464679914735E-16,0.,1.));
#8133=DIRECTION('center_axis',(0.,1.,0.));
#8134=DIRECTION('ref_axis',(1.,0.,0.));
#8135=DIRECTION('center_axis',(0.,1.,0.));
#8136=DIRECTION('ref_axis',(1.,0.,0.));
#8137=DIRECTION('center_axis',(0.,-1.,0.));
#8138=DIRECTION('ref_axis',(1.,0.,0.));
#8139=DIRECTION('center_axis',(0.,-1.,0.));
#8140=DIRECTION('ref_axis',(1.,0.,0.));
#8141=DIRECTION('',(0.,1.,0.));
#8142=DIRECTION('center_axis',(0.,1.,0.));
#8143=DIRECTION('ref_axis',(0.,0.,1.));
#8144=DIRECTION('center_axis',(0.,-1.,0.));
#8145=DIRECTION('ref_axis',(1.,0.,0.));
#8146=DIRECTION('center_axis',(0.,-1.,0.));
#8147=DIRECTION('ref_axis',(1.,0.,0.));
#8148=DIRECTION('center_axis',(0.,-1.,0.));
#8149=DIRECTION('ref_axis',(1.,0.,0.));
#8150=DIRECTION('center_axis',(0.,-1.,0.));
#8151=DIRECTION('ref_axis',(1.,0.,0.));
#8152=DIRECTION('',(0.707106781186548,0.707106781186547,8.65956056235494E-17));
#8153=DIRECTION('center_axis',(0.,-1.,0.));
#8154=DIRECTION('ref_axis',(1.,0.,0.));
#8155=DIRECTION('center_axis',(0.,-1.,0.));
#8156=DIRECTION('ref_axis',(1.,0.,0.));
#8157=DIRECTION('',(0.,1.,0.));
#8158=DIRECTION('center_axis',(0.,1.,0.));
#8159=DIRECTION('ref_axis',(1.,0.,0.));
#8160=DIRECTION('center_axis',(0.,-1.,0.));
#8161=DIRECTION('ref_axis',(1.,0.,0.));
#8162=DIRECTION('',(-0.707106781186548,0.707106781186547,-8.65956056235494E-17));
#8163=DIRECTION('center_axis',(0.,-1.,0.));
#8164=DIRECTION('ref_axis',(0.,0.,-1.));
#8165=DIRECTION('center_axis',(0.,-1.,0.));
#8166=DIRECTION('ref_axis',(1.,0.,0.));
#8167=DIRECTION('',(0.,1.,0.));
#8168=DIRECTION('axis',(0.,0.,1.));
#8169=DIRECTION('refdir',(1.,0.,0.));
#8170=DIRECTION('center_axis',(0.,0.,1.));
#8171=DIRECTION('ref_axis',(1.,0.,0.));
#8172=DIRECTION('center_axis',(1.22464679914735E-16,-1.,0.));
#8173=DIRECTION('ref_axis',(-1.,-1.22464679914735E-16,0.));
#8174=DIRECTION('center_axis',(0.707106781186548,0.,0.707106781186548));
#8175=DIRECTION('ref_axis',(0.707106781186548,0.,-0.707106781186548));
#8176=DIRECTION('center_axis',(8.65956056235494E-17,-1.,-8.65956056235493E-17));
#8177=DIRECTION('ref_axis',(-0.707106781186547,-1.22464679914735E-16,0.707106781186547));
#8178=DIRECTION('center_axis',(1.,0.,0.));
#8179=DIRECTION('ref_axis',(6.12323399573676E-17,0.,-1.));
#8180=DIRECTION('center_axis',(7.49879891330929E-33,-1.,-1.22464679914735E-16));
#8181=DIRECTION('ref_axis',(-6.12323399573676E-17,-1.22464679914735E-16,
1.));
#8182=DIRECTION('center_axis',(0.707106781186548,0.,-0.707106781186548));
#8183=DIRECTION('ref_axis',(-0.707106781186548,0.,-0.707106781186548));
#8184=DIRECTION('center_axis',(-8.65956056235493E-17,-1.,-8.65956056235494E-17));
#8185=DIRECTION('ref_axis',(0.707106781186547,-1.22464679914735E-16,0.707106781186547));
#8186=DIRECTION('center_axis',(0.,0.,-1.));
#8187=DIRECTION('ref_axis',(-1.,0.,-1.22464679914735E-16));
#8188=DIRECTION('center_axis',(-1.22464679914735E-16,-1.,-1.49975978266186E-32));
#8189=DIRECTION('ref_axis',(1.,-1.22464679914735E-16,1.22464679914735E-16));
#8190=DIRECTION('center_axis',(-0.707106781186547,0.,-0.707106781186548));
#8191=DIRECTION('ref_axis',(-0.707106781186548,0.,0.707106781186547));
#8192=DIRECTION('center_axis',(-8.65956056235493E-17,-1.,8.65956056235493E-17));
#8193=DIRECTION('ref_axis',(0.707106781186548,-1.22464679914735E-16,-0.707106781186547));
#8194=DIRECTION('center_axis',(-1.,0.,0.));
#8195=DIRECTION('ref_axis',(-1.83697019872103E-16,0.,1.));
#8196=DIRECTION('center_axis',(-2.24963967399279E-32,-1.,1.22464679914735E-16));
#8197=DIRECTION('ref_axis',(1.83697019872103E-16,-1.22464679914735E-16,
-1.));
#8198=DIRECTION('center_axis',(-0.707106781186548,0.,0.707106781186548));
#8199=DIRECTION('ref_axis',(0.707106781186547,0.,0.707106781186548));
#8200=DIRECTION('center_axis',(8.65956056235493E-17,-1.,8.65956056235493E-17));
#8201=DIRECTION('ref_axis',(-0.707106781186547,-1.22464679914735E-16,-0.707106781186548));
#8202=DIRECTION('axis',(0.,0.,1.));
#8203=DIRECTION('refdir',(1.,0.,0.));
#8204=DIRECTION('center_axis',(0.,0.,1.));
#8205=DIRECTION('ref_axis',(1.,0.,0.));
#8206=DIRECTION('center_axis',(0.,-1.,0.));
#8207=DIRECTION('ref_axis',(0.,0.,-1.));
#8208=DIRECTION('center_axis',(0.,-1.,0.));
#8209=DIRECTION('ref_axis',(0.,0.,-1.));
#8210=DIRECTION('center_axis',(0.,1.,0.));
#8211=DIRECTION('ref_axis',(1.,0.,0.));
#8212=DIRECTION('center_axis',(0.,1.,0.));
#8213=DIRECTION('ref_axis',(1.,0.,0.));
#8214=DIRECTION('center_axis',(0.,1.,0.));
#8215=DIRECTION('ref_axis',(1.,0.,0.));
#8216=DIRECTION('center_axis',(0.,1.,0.));
#8217=DIRECTION('ref_axis',(1.,0.,0.));
#8218=DIRECTION('',(0.,-1.,0.));
#8219=DIRECTION('center_axis',(0.,-1.,0.));
#8220=DIRECTION('ref_axis',(1.,0.,0.));
#8221=DIRECTION('center_axis',(0.,1.,0.));
#8222=DIRECTION('ref_axis',(1.,0.,0.));
#8223=DIRECTION('center_axis',(0.,1.,0.));
#8224=DIRECTION('ref_axis',(1.,0.,0.));
#8225=DIRECTION('center_axis',(0.,1.,0.));
#8226=DIRECTION('ref_axis',(1.,0.,0.));
#8227=DIRECTION('center_axis',(0.,1.,0.));
#8228=DIRECTION('ref_axis',(1.,0.,0.));
#8229=DIRECTION('center_axis',(0.,1.,0.));
#8230=DIRECTION('ref_axis',(1.,0.,0.));
#8231=DIRECTION('center_axis',(0.,1.,0.));
#8232=DIRECTION('ref_axis',(1.,0.,0.));
#8233=DIRECTION('center_axis',(0.,-1.,0.));
#8234=DIRECTION('ref_axis',(1.,0.,0.));
#8235=DIRECTION('center_axis',(0.,-1.,0.));
#8236=DIRECTION('ref_axis',(0.,0.,-1.));
#8237=DIRECTION('center_axis',(6.12323399573677E-17,0.,1.));
#8238=DIRECTION('ref_axis',(1.,0.,0.));
#8239=DIRECTION('center_axis',(0.,-1.,0.));
#8240=DIRECTION('ref_axis',(0.,0.,-1.));
#8241=DIRECTION('center_axis',(0.,1.,0.));
#8242=DIRECTION('ref_axis',(1.,0.,0.));
#8243=DIRECTION('center_axis',(0.,-1.,0.));
#8244=DIRECTION('ref_axis',(1.,0.,0.));
#8245=DIRECTION('center_axis',(0.,-1.,0.));
#8246=DIRECTION('ref_axis',(0.,0.,-1.));
#8247=DIRECTION('center_axis',(0.,0.,1.));
#8248=DIRECTION('ref_axis',(1.,0.,0.));
#8249=DIRECTION('center_axis',(0.,-1.,0.));
#8250=DIRECTION('ref_axis',(0.,0.,-1.));
#8251=DIRECTION('center_axis',(0.,1.,0.));
#8252=DIRECTION('ref_axis',(1.,0.,0.));
#8253=DIRECTION('center_axis',(0.,-1.,0.));
#8254=DIRECTION('ref_axis',(1.,0.,0.));
#8255=DIRECTION('center_axis',(0.,-1.,0.));
#8256=DIRECTION('ref_axis',(0.,0.,-1.));
#8257=DIRECTION('center_axis',(0.,0.,1.));
#8258=DIRECTION('ref_axis',(1.,0.,0.));
#8259=DIRECTION('center_axis',(0.,-1.,0.));
#8260=DIRECTION('ref_axis',(0.,0.,-1.));
#8261=DIRECTION('center_axis',(0.,1.,0.));
#8262=DIRECTION('ref_axis',(1.,0.,0.));
#8263=DIRECTION('center_axis',(0.,-1.,0.));
#8264=DIRECTION('ref_axis',(1.,0.,0.));
#8265=DIRECTION('center_axis',(0.,-1.,0.));
#8266=DIRECTION('ref_axis',(0.,0.,-1.));
#8267=DIRECTION('center_axis',(0.,0.,1.));
#8268=DIRECTION('ref_axis',(1.,0.,0.));
#8269=DIRECTION('center_axis',(0.,-1.,0.));
#8270=DIRECTION('ref_axis',(0.,0.,-1.));
#8271=DIRECTION('center_axis',(0.,1.,0.));
#8272=DIRECTION('ref_axis',(1.,0.,0.));
#8273=DIRECTION('center_axis',(0.,-1.,0.));
#8274=DIRECTION('ref_axis',(1.,0.,0.));
#8275=DIRECTION('center_axis',(0.,-1.,0.));
#8276=DIRECTION('ref_axis',(0.,0.,-1.));
#8277=DIRECTION('center_axis',(6.12323399573676E-17,0.,1.));
#8278=DIRECTION('ref_axis',(1.,0.,0.));
#8279=DIRECTION('center_axis',(0.,-1.,0.));
#8280=DIRECTION('ref_axis',(0.,0.,-1.));
#8281=DIRECTION('center_axis',(0.,1.,0.));
#8282=DIRECTION('ref_axis',(1.,0.,0.));
#8283=DIRECTION('center_axis',(0.,-1.,0.));
#8284=DIRECTION('ref_axis',(1.,0.,0.));
#8285=DIRECTION('center_axis',(0.,-1.,0.));
#8286=DIRECTION('ref_axis',(0.,0.,-1.));
#8287=DIRECTION('center_axis',(0.,0.,1.));
#8288=DIRECTION('ref_axis',(1.,0.,0.));
#8289=DIRECTION('center_axis',(0.,-1.,0.));
#8290=DIRECTION('ref_axis',(0.,0.,-1.));
#8291=DIRECTION('center_axis',(0.,1.,0.));
#8292=DIRECTION('ref_axis',(1.,0.,0.));
#8293=DIRECTION('center_axis',(0.,1.,0.));
#8294=DIRECTION('ref_axis',(1.,0.,0.));
#8295=DIRECTION('',(0.,1.,0.));
#8296=DIRECTION('center_axis',(0.,-1.,0.));
#8297=DIRECTION('ref_axis',(1.,0.,0.));
#8298=DIRECTION('center_axis',(0.,-1.,0.));
#8299=DIRECTION('ref_axis',(1.,0.,0.));
#8300=DIRECTION('center_axis',(0.,1.,0.));
#8301=DIRECTION('ref_axis',(1.,0.,0.));
#8302=DIRECTION('center_axis',(0.,-1.,0.));
#8303=DIRECTION('ref_axis',(0.,0.,-1.));
#8304=DIRECTION('center_axis',(0.,0.,1.));
#8305=DIRECTION('ref_axis',(1.,0.,0.));
#8306=DIRECTION('center_axis',(0.,-1.,0.));
#8307=DIRECTION('ref_axis',(0.,0.,-1.));
#8308=DIRECTION('center_axis',(0.,-1.,0.));
#8309=DIRECTION('ref_axis',(-1.,0.,0.));
#8310=DIRECTION('center_axis',(0.,1.,0.));
#8311=DIRECTION('ref_axis',(1.,0.,0.));
#8312=DIRECTION('axis',(0.,0.,1.));
#8313=DIRECTION('refdir',(1.,0.,0.));
#8314=DIRECTION('center_axis',(0.,1.,0.));
#8315=DIRECTION('ref_axis',(0.,0.,1.));
#8316=DIRECTION('center_axis',(0.,-1.,0.));
#8317=DIRECTION('ref_axis',(1.,0.,0.));
#8318=DIRECTION('center_axis',(0.,-1.,0.));
#8319=DIRECTION('ref_axis',(1.,0.,0.));
#8320=DIRECTION('center_axis',(0.,-1.,0.));
#8321=DIRECTION('ref_axis',(1.,0.,0.));
#8322=DIRECTION('center_axis',(0.,-1.,0.));
#8323=DIRECTION('ref_axis',(1.,0.,0.));
#8324=DIRECTION('',(0.,1.,0.));
#8325=DIRECTION('center_axis',(0.,-1.,0.));
#8326=DIRECTION('ref_axis',(0.,0.,-1.));
#8327=DIRECTION('center_axis',(0.,-1.,0.));
#8328=DIRECTION('ref_axis',(1.,0.,0.));
#8329=DIRECTION('center_axis',(0.,-1.,0.));
#8330=DIRECTION('ref_axis',(1.,0.,0.));
#8331=DIRECTION('',(0.,1.,0.));
#8332=DIRECTION('center_axis',(0.,1.,0.));
#8333=DIRECTION('ref_axis',(0.,0.,1.));
#8334=DIRECTION('center_axis',(0.,-1.,0.));
#8335=DIRECTION('ref_axis',(1.,0.,0.));
#8336=DIRECTION('center_axis',(0.,-1.,0.));
#8337=DIRECTION('ref_axis',(1.,0.,0.));
#8338=DIRECTION('center_axis',(0.,-1.,0.));
#8339=DIRECTION('ref_axis',(1.,0.,0.));
#8340=DIRECTION('center_axis',(0.,-1.,0.));
#8341=DIRECTION('ref_axis',(1.,0.,0.));
#8342=DIRECTION('',(0.,1.,0.));
#8343=DIRECTION('center_axis',(0.,-1.,0.));
#8344=DIRECTION('ref_axis',(0.,0.,-1.));
#8345=DIRECTION('center_axis',(0.,-1.,0.));
#8346=DIRECTION('ref_axis',(1.,0.,0.));
#8347=DIRECTION('center_axis',(0.,-1.,0.));
#8348=DIRECTION('ref_axis',(1.,0.,0.));
#8349=DIRECTION('',(0.,1.,0.));
#8350=DIRECTION('',(0.,0.,1.));
#8351=DIRECTION('',(1.,0.,0.));
#8352=DIRECTION('',(0.,0.,1.));
#8353=DIRECTION('',(1.,0.,0.));
#8354=DIRECTION('',(0.,0.,1.));
#8355=DIRECTION('',(1.,0.,0.));
#8356=DIRECTION('',(0.,0.,1.));
#8357=DIRECTION('',(1.,0.,0.));
#8358=DIRECTION('',(0.,0.,1.));
#8359=DIRECTION('',(1.,0.,0.));
#8360=DIRECTION('axis',(0.,0.,1.));
#8361=DIRECTION('refdir',(1.,0.,0.));
#8362=DIRECTION('axis',(0.,0.,1.));
#8363=DIRECTION('refdir',(1.,0.,0.));
#8364=DIRECTION('center_axis',(0.,0.,1.));
#8365=DIRECTION('ref_axis',(1.,0.,0.));
#8366=DIRECTION('center_axis',(0.,0.,1.));
#8367=DIRECTION('ref_axis',(1.,0.,0.));
#8368=DIRECTION('',(0.,0.,1.));
#8369=DIRECTION('center_axis',(0.,0.,-1.));
#8370=DIRECTION('ref_axis',(1.,0.,0.));
#8371=DIRECTION('center_axis',(0.,0.,1.));
#8372=DIRECTION('ref_axis',(1.,0.,0.));
#8373=DIRECTION('center_axis',(0.,0.,1.));
#8374=DIRECTION('ref_axis',(1.,0.,0.));
#8375=DIRECTION('center_axis',(0.,0.,1.));
#8376=DIRECTION('ref_axis',(1.,0.,0.));
#8377=DIRECTION('',(0.,0.,1.));
#8378=DIRECTION('center_axis',(0.,0.,-1.));
#8379=DIRECTION('ref_axis',(1.,0.,0.));
#8380=DIRECTION('center_axis',(0.,0.,1.));
#8381=DIRECTION('ref_axis',(-0.162294462269189,0.986742371400334,0.));
#8382=DIRECTION('',(0.,0.,1.));
#8383=DIRECTION('center_axis',(0.,0.,1.));
#8384=DIRECTION('ref_axis',(1.,0.,0.));
#8385=DIRECTION('',(0.,0.,-1.));
#8386=DIRECTION('center_axis',(0.,0.,1.));
#8387=DIRECTION('ref_axis',(1.,0.,0.));
#8388=DIRECTION('center_axis',(0.986742371400334,0.162294462269189,0.));
#8389=DIRECTION('ref_axis',(-0.162294462269189,0.986742371400334,0.));
#8390=DIRECTION('',(-0.162294462269189,0.986742371400334,0.));
#8391=DIRECTION('',(0.,0.,1.));
#8392=DIRECTION('',(0.162294462269189,-0.986742371400334,0.));
#8393=DIRECTION('center_axis',(0.,0.,1.));
#8394=DIRECTION('ref_axis',(1.,0.,0.));
#8395=DIRECTION('',(0.162294462269189,-0.986742371400334,0.));
#8396=DIRECTION('center_axis',(0.,0.,1.));
#8397=DIRECTION('ref_axis',(1.,0.,0.));
#8398=DIRECTION('center_axis',(0.,0.,1.));
#8399=DIRECTION('ref_axis',(1.,0.,0.));
#8400=DIRECTION('center_axis',(-0.986742371400334,-0.162294462269189,0.));
#8401=DIRECTION('ref_axis',(0.162294462269189,-0.986742371400334,0.));
#8402=DIRECTION('',(-0.162294462269189,0.986742371400334,0.));
#8403=DIRECTION('',(0.,0.,-1.));
#8404=DIRECTION('center_axis',(0.,0.,1.));
#8405=DIRECTION('ref_axis',(0.162294462269189,-0.986742371400334,0.));
#8406=DIRECTION('center_axis',(0.,0.,1.));
#8407=DIRECTION('ref_axis',(1.,0.,0.));
#8408=DIRECTION('center_axis',(0.,0.,1.));
#8409=DIRECTION('ref_axis',(1.,0.,0.));
#8410=DIRECTION('center_axis',(0.,0.,1.));
#8411=DIRECTION('ref_axis',(1.,0.,0.));
#8412=DIRECTION('center_axis',(0.,0.,1.));
#8413=DIRECTION('ref_axis',(1.,0.,0.));
#8414=DIRECTION('center_axis',(0.,0.,1.));
#8415=DIRECTION('ref_axis',(1.,0.,0.));
#8416=DIRECTION('center_axis',(0.,0.,-1.));
#8417=DIRECTION('ref_axis',(1.,0.,0.));
#8418=DIRECTION('center_axis',(0.,0.,1.));
#8419=DIRECTION('ref_axis',(1.,0.,0.));
#8420=DIRECTION('',(0.,0.,-1.));
#8421=DIRECTION('center_axis',(0.,0.,1.));
#8422=DIRECTION('ref_axis',(1.,0.,0.));
#8423=DIRECTION('',(0.,0.,-1.));
#8424=DIRECTION('center_axis',(0.,0.,1.));
#8425=DIRECTION('ref_axis',(1.,0.,0.));
#8426=DIRECTION('center_axis',(0.,0.,1.));
#8427=DIRECTION('ref_axis',(1.,0.,0.));
#8428=DIRECTION('center_axis',(0.,0.,1.));
#8429=DIRECTION('ref_axis',(1.,0.,0.));
#8430=DIRECTION('',(0.,0.,-1.));
#8431=DIRECTION('center_axis',(0.,0.,1.));
#8432=DIRECTION('ref_axis',(1.,0.,0.));
#8433=DIRECTION('center_axis',(0.,0.,1.));
#8434=DIRECTION('ref_axis',(1.,0.,0.));
#8435=DIRECTION('axis',(0.,0.,1.));
#8436=DIRECTION('refdir',(1.,0.,0.));
#8437=DIRECTION('center_axis',(0.,0.,1.));
#8438=DIRECTION('ref_axis',(1.,0.,0.));
#8439=DIRECTION('center_axis',(0.,0.,-1.));
#8440=DIRECTION('ref_axis',(1.,0.,0.));
#8441=DIRECTION('',(0.,0.,-1.));
#8442=DIRECTION('center_axis',(0.,0.,-1.));
#8443=DIRECTION('ref_axis',(1.,0.,0.));
#8444=DIRECTION('center_axis',(0.,0.,1.));
#8445=DIRECTION('ref_axis',(1.,0.,0.));
#8446=DIRECTION('center_axis',(0.,0.,1.));
#8447=DIRECTION('ref_axis',(1.,0.,0.));
#8448=DIRECTION('',(0.,0.,-1.));
#8449=DIRECTION('center_axis',(0.,0.,1.));
#8450=DIRECTION('ref_axis',(1.,0.,0.));
#8451=DIRECTION('center_axis',(0.,0.,1.));
#8452=DIRECTION('ref_axis',(1.,0.,0.));
#8453=DIRECTION('center_axis',(0.,0.,1.));
#8454=DIRECTION('ref_axis',(1.,0.,0.));
#8455=DIRECTION('axis',(0.,0.,1.));
#8456=DIRECTION('refdir',(1.,0.,0.));
#8457=DIRECTION('center_axis',(0.,0.,1.));
#8458=DIRECTION('ref_axis',(1.,0.,0.));
#8459=DIRECTION('center_axis',(0.,0.,-1.));
#8460=DIRECTION('ref_axis',(1.,0.,0.));
#8461=DIRECTION('',(0.,0.,-1.));
#8462=DIRECTION('center_axis',(0.,0.,-1.));
#8463=DIRECTION('ref_axis',(1.,0.,0.));
#8464=DIRECTION('center_axis',(0.,0.,1.));
#8465=DIRECTION('ref_axis',(1.,0.,0.));
#8466=DIRECTION('center_axis',(0.,0.,1.));
#8467=DIRECTION('ref_axis',(1.,0.,0.));
#8468=DIRECTION('',(0.,0.,-1.));
#8469=DIRECTION('center_axis',(0.,0.,1.));
#8470=DIRECTION('ref_axis',(1.,0.,0.));
#8471=DIRECTION('center_axis',(0.,0.,1.));
#8472=DIRECTION('ref_axis',(1.,0.,0.));
#8473=DIRECTION('center_axis',(0.,0.,1.));
#8474=DIRECTION('ref_axis',(1.,0.,0.));
#8475=DIRECTION('axis',(0.,0.,1.));
#8476=DIRECTION('refdir',(1.,0.,0.));
#8477=DIRECTION('center_axis',(1.,0.,0.));
#8478=DIRECTION('ref_axis',(0.,0.,-1.));
#8479=DIRECTION('',(0.,0.,1.));
#8480=DIRECTION('center_axis',(1.,0.,0.));
#8481=DIRECTION('ref_axis',(0.,0.,-1.));
#8482=DIRECTION('center_axis',(1.,0.,0.));
#8483=DIRECTION('ref_axis',(0.,0.,-1.));
#8484=DIRECTION('center_axis',(1.,0.,0.));
#8485=DIRECTION('ref_axis',(0.,0.,-1.));
#8486=DIRECTION('',(1.,0.,0.));
#8487=DIRECTION('center_axis',(1.,0.,0.));
#8488=DIRECTION('ref_axis',(0.,0.,-1.));
#8489=DIRECTION('',(0.,0.,-1.));
#8490=DIRECTION('center_axis',(0.,0.,1.));
#8491=DIRECTION('ref_axis',(1.,0.,0.));
#8492=DIRECTION('center_axis',(0.,0.,-1.));
#8493=DIRECTION('ref_axis',(1.,0.,0.));
#8494=DIRECTION('',(0.,0.,-1.));
#8495=DIRECTION('center_axis',(0.,0.,-1.));
#8496=DIRECTION('ref_axis',(1.,0.,0.));
#8497=DIRECTION('center_axis',(0.,0.,1.));
#8498=DIRECTION('ref_axis',(1.,0.,0.));
#8499=DIRECTION('center_axis',(0.,0.,1.));
#8500=DIRECTION('ref_axis',(1.,0.,0.));
#8501=DIRECTION('',(0.,0.,-1.));
#8502=DIRECTION('center_axis',(0.,0.,1.));
#8503=DIRECTION('ref_axis',(1.,0.,0.));
#8504=DIRECTION('center_axis',(0.,0.,1.));
#8505=DIRECTION('ref_axis',(1.,0.,0.));
#8506=DIRECTION('center_axis',(0.,0.,1.));
#8507=DIRECTION('ref_axis',(1.,0.,0.));
#8508=DIRECTION('axis',(0.,0.,1.));
#8509=DIRECTION('refdir',(1.,0.,0.));
#8510=DIRECTION('center_axis',(1.,0.,0.));
#8511=DIRECTION('ref_axis',(0.,0.,-1.));
#8512=DIRECTION('',(0.,0.,1.));
#8513=DIRECTION('center_axis',(1.,0.,0.));
#8514=DIRECTION('ref_axis',(0.,0.,-1.));
#8515=DIRECTION('center_axis',(1.,0.,0.));
#8516=DIRECTION('ref_axis',(0.,0.,-1.));
#8517=DIRECTION('center_axis',(1.,0.,0.));
#8518=DIRECTION('ref_axis',(0.,0.,-1.));
#8519=DIRECTION('',(1.,0.,0.));
#8520=DIRECTION('center_axis',(1.,0.,0.));
#8521=DIRECTION('ref_axis',(0.,0.,-1.));
#8522=DIRECTION('',(0.,0.,-1.));
#8523=DIRECTION('center_axis',(0.,0.,1.));
#8524=DIRECTION('ref_axis',(1.,0.,0.));
#8525=DIRECTION('center_axis',(0.,0.,-1.));
#8526=DIRECTION('ref_axis',(1.,0.,0.));
#8527=DIRECTION('',(0.,0.,-1.));
#8528=DIRECTION('center_axis',(0.,0.,-1.));
#8529=DIRECTION('ref_axis',(1.,0.,0.));
#8530=DIRECTION('center_axis',(0.,0.,1.));
#8531=DIRECTION('ref_axis',(1.,0.,0.));
#8532=DIRECTION('center_axis',(0.,0.,1.));
#8533=DIRECTION('ref_axis',(1.,0.,0.));
#8534=DIRECTION('',(0.,0.,-1.));
#8535=DIRECTION('center_axis',(0.,0.,1.));
#8536=DIRECTION('ref_axis',(1.,0.,0.));
#8537=DIRECTION('center_axis',(0.,0.,1.));
#8538=DIRECTION('ref_axis',(1.,0.,0.));
#8539=DIRECTION('center_axis',(0.,0.,1.));
#8540=DIRECTION('ref_axis',(1.,0.,0.));
#8541=DIRECTION('axis',(0.,0.,1.));
#8542=DIRECTION('refdir',(1.,0.,0.));
#8543=DIRECTION('center_axis',(0.,0.,1.));
#8544=DIRECTION('ref_axis',(1.,0.,0.));
#8545=DIRECTION('center_axis',(0.,0.,-1.));
#8546=DIRECTION('ref_axis',(1.,0.,0.));
#8547=DIRECTION('',(0.,0.,-1.));
#8548=DIRECTION('center_axis',(0.,0.,-1.));
#8549=DIRECTION('ref_axis',(1.,0.,0.));
#8550=DIRECTION('center_axis',(0.,0.,1.));
#8551=DIRECTION('ref_axis',(1.,0.,0.));
#8552=DIRECTION('center_axis',(0.,0.,1.));
#8553=DIRECTION('ref_axis',(1.,0.,0.));
#8554=DIRECTION('',(0.,0.,-1.));
#8555=DIRECTION('center_axis',(0.,0.,1.));
#8556=DIRECTION('ref_axis',(1.,0.,0.));
#8557=DIRECTION('center_axis',(0.,0.,1.));
#8558=DIRECTION('ref_axis',(1.,0.,0.));
#8559=DIRECTION('center_axis',(0.,0.,1.));
#8560=DIRECTION('ref_axis',(1.,0.,0.));
#8561=DIRECTION('axis',(0.,0.,1.));
#8562=DIRECTION('refdir',(1.,0.,0.));
#8563=DIRECTION('center_axis',(0.,0.,1.));
#8564=DIRECTION('ref_axis',(1.,0.,0.));
#8565=DIRECTION('center_axis',(0.,0.,1.));
#8566=DIRECTION('ref_axis',(1.,0.,0.));
#8567=DIRECTION('',(0.,0.,1.));
#8568=DIRECTION('center_axis',(0.,0.,-1.));
#8569=DIRECTION('ref_axis',(1.,0.,0.));
#8570=DIRECTION('center_axis',(0.,0.,1.));
#8571=DIRECTION('ref_axis',(1.,0.,0.));
#8572=DIRECTION('center_axis',(0.,0.,1.));
#8573=DIRECTION('ref_axis',(1.,0.,0.));
#8574=DIRECTION('center_axis',(0.,0.,1.));
#8575=DIRECTION('ref_axis',(1.,0.,0.));
#8576=DIRECTION('',(0.,0.,1.));
#8577=DIRECTION('center_axis',(0.,0.,1.));
#8578=DIRECTION('ref_axis',(1.,0.,0.));
#8579=DIRECTION('center_axis',(0.,0.,1.));
#8580=DIRECTION('ref_axis',(1.,0.,0.));
#8581=DIRECTION('center_axis',(0.,0.,1.));
#8582=DIRECTION('ref_axis',(1.,0.,0.));
#8583=DIRECTION('center_axis',(0.,0.,1.));
#8584=DIRECTION('ref_axis',(1.,0.,0.));
#8585=DIRECTION('center_axis',(0.,0.,1.));
#8586=DIRECTION('ref_axis',(1.,0.,0.));
#8587=DIRECTION('center_axis',(0.,0.,1.));
#8588=DIRECTION('ref_axis',(1.,0.,0.));
#8589=DIRECTION('center_axis',(0.,0.,1.));
#8590=DIRECTION('ref_axis',(1.,0.,0.));
#8591=DIRECTION('center_axis',(0.,0.,-1.));
#8592=DIRECTION('ref_axis',(1.,0.,0.));
#8593=DIRECTION('center_axis',(0.,0.,1.));
#8594=DIRECTION('ref_axis',(1.,0.,0.));
#8595=DIRECTION('',(0.,0.,-1.));
#8596=DIRECTION('center_axis',(0.,0.,1.));
#8597=DIRECTION('ref_axis',(1.,0.,0.));
#8598=DIRECTION('',(0.,0.,-1.));
#8599=DIRECTION('center_axis',(0.,0.,1.));
#8600=DIRECTION('ref_axis',(1.,0.,0.));
#8601=DIRECTION('center_axis',(0.,0.,1.));
#8602=DIRECTION('ref_axis',(1.,0.,0.));
#8603=DIRECTION('center_axis',(0.,0.,1.));
#8604=DIRECTION('ref_axis',(1.,0.,0.));
#8605=DIRECTION('',(0.,0.,-1.));
#8606=DIRECTION('center_axis',(0.,0.,1.));
#8607=DIRECTION('ref_axis',(1.,0.,0.));
#8608=DIRECTION('center_axis',(0.,0.,1.));
#8609=DIRECTION('ref_axis',(1.,0.,0.));
#8610=DIRECTION('axis',(0.,0.,1.));
#8611=DIRECTION('refdir',(1.,0.,0.));
#8612=DIRECTION('center_axis',(0.,0.,1.));
#8613=DIRECTION('ref_axis',(1.,0.,0.));
#8614=DIRECTION('center_axis',(0.,0.,-1.));
#8615=DIRECTION('ref_axis',(1.,0.,0.));
#8616=DIRECTION('',(0.,0.,-1.));
#8617=DIRECTION('center_axis',(0.,0.,-1.));
#8618=DIRECTION('ref_axis',(1.,0.,0.));
#8619=DIRECTION('center_axis',(0.,0.,1.));
#8620=DIRECTION('ref_axis',(1.,0.,0.));
#8621=DIRECTION('center_axis',(0.,0.,1.));
#8622=DIRECTION('ref_axis',(1.,0.,0.));
#8623=DIRECTION('',(0.,0.,-1.));
#8624=DIRECTION('center_axis',(0.,0.,1.));
#8625=DIRECTION('ref_axis',(1.,0.,0.));
#8626=DIRECTION('center_axis',(0.,0.,1.));
#8627=DIRECTION('ref_axis',(1.,0.,0.));
#8628=DIRECTION('center_axis',(0.,0.,1.));
#8629=DIRECTION('ref_axis',(1.,0.,0.));
#8630=DIRECTION('axis',(0.,0.,1.));
#8631=DIRECTION('refdir',(1.,0.,0.));
#8632=DIRECTION('center_axis',(0.,0.,1.));
#8633=DIRECTION('ref_axis',(1.,0.,0.));
#8634=DIRECTION('center_axis',(0.,0.,-1.));
#8635=DIRECTION('ref_axis',(1.,0.,0.));
#8636=DIRECTION('',(0.,0.,-1.));
#8637=DIRECTION('center_axis',(0.,0.,-1.));
#8638=DIRECTION('ref_axis',(1.,0.,0.));
#8639=DIRECTION('center_axis',(0.,0.,1.));
#8640=DIRECTION('ref_axis',(1.,0.,0.));
#8641=DIRECTION('center_axis',(0.,0.,1.));
#8642=DIRECTION('ref_axis',(1.,0.,0.));
#8643=DIRECTION('',(0.,0.,-1.));
#8644=DIRECTION('center_axis',(0.,0.,1.));
#8645=DIRECTION('ref_axis',(1.,0.,0.));
#8646=DIRECTION('center_axis',(0.,0.,1.));
#8647=DIRECTION('ref_axis',(1.,0.,0.));
#8648=DIRECTION('center_axis',(0.,0.,1.));
#8649=DIRECTION('ref_axis',(1.,0.,0.));
#8650=DIRECTION('axis',(0.,0.,1.));
#8651=DIRECTION('refdir',(1.,0.,0.));
#8652=DIRECTION('center_axis',(0.,0.,1.));
#8653=DIRECTION('ref_axis',(1.,0.,0.));
#8654=DIRECTION('center_axis',(0.,0.,-1.));
#8655=DIRECTION('ref_axis',(1.,0.,0.));
#8656=DIRECTION('',(0.,0.,-1.));
#8657=DIRECTION('center_axis',(0.,0.,-1.));
#8658=DIRECTION('ref_axis',(1.,0.,0.));
#8659=DIRECTION('center_axis',(0.,0.,1.));
#8660=DIRECTION('ref_axis',(1.,0.,0.));
#8661=DIRECTION('center_axis',(0.,0.,1.));
#8662=DIRECTION('ref_axis',(1.,0.,0.));
#8663=DIRECTION('',(0.,0.,-1.));
#8664=DIRECTION('center_axis',(0.,0.,1.));
#8665=DIRECTION('ref_axis',(1.,0.,0.));
#8666=DIRECTION('center_axis',(0.,0.,1.));
#8667=DIRECTION('ref_axis',(1.,0.,0.));
#8668=DIRECTION('center_axis',(0.,0.,1.));
#8669=DIRECTION('ref_axis',(1.,0.,0.));
#8670=DIRECTION('axis',(0.,0.,1.));
#8671=DIRECTION('refdir',(1.,0.,0.));
#8672=DIRECTION('center_axis',(0.,0.,1.));
#8673=DIRECTION('ref_axis',(1.,0.,0.));
#8674=DIRECTION('center_axis',(0.,0.,-1.));
#8675=DIRECTION('ref_axis',(1.,0.,0.));
#8676=DIRECTION('',(0.,0.,-1.));
#8677=DIRECTION('center_axis',(0.,0.,-1.));
#8678=DIRECTION('ref_axis',(1.,0.,0.));
#8679=DIRECTION('center_axis',(0.,0.,1.));
#8680=DIRECTION('ref_axis',(1.,0.,0.));
#8681=DIRECTION('center_axis',(0.,0.,1.));
#8682=DIRECTION('ref_axis',(1.,0.,0.));
#8683=DIRECTION('',(0.,0.,-1.));
#8684=DIRECTION('center_axis',(0.,0.,1.));
#8685=DIRECTION('ref_axis',(1.,0.,0.));
#8686=DIRECTION('center_axis',(0.,0.,1.));
#8687=DIRECTION('ref_axis',(1.,0.,0.));
#8688=DIRECTION('center_axis',(0.,0.,1.));
#8689=DIRECTION('ref_axis',(1.,0.,0.));
#8690=DIRECTION('axis',(0.,0.,1.));
#8691=DIRECTION('refdir',(1.,0.,0.));
#8692=DIRECTION('center_axis',(0.866025403784439,0.,-0.5));
#8693=DIRECTION('ref_axis',(0.5,0.,0.866025403784439));
#8694=DIRECTION('',(0.5,0.,0.866025403784439));
#8695=DIRECTION('',(0.,-1.,0.));
#8696=DIRECTION('',(0.5,0.,0.866025403784439));
#8697=DIRECTION('',(0.,-1.,0.));
#8698=DIRECTION('center_axis',(1.20185167898973E-16,0.,-1.));
#8699=DIRECTION('ref_axis',(1.,0.,1.20185167898973E-16));
#8700=DIRECTION('',(1.,0.,1.20185167898973E-16));
#8701=DIRECTION('',(0.,-1.,0.));
#8702=DIRECTION('',(1.,0.,1.20185167898973E-16));
#8703=DIRECTION('center_axis',(-0.866025403784439,0.,-0.5));
#8704=DIRECTION('ref_axis',(0.5,0.,-0.866025403784439));
#8705=DIRECTION('',(0.5,0.,-0.866025403784439));
#8706=DIRECTION('',(0.,-1.,0.));
#8707=DIRECTION('',(0.5,0.,-0.866025403784439));
#8708=DIRECTION('center_axis',(-0.866025403784439,0.,0.5));
#8709=DIRECTION('ref_axis',(-0.5,0.,-0.866025403784439));
#8710=DIRECTION('',(-0.5,0.,-0.866025403784439));
#8711=DIRECTION('',(0.,-1.,0.));
#8712=DIRECTION('',(-0.5,0.,-0.866025403784439));
#8713=DIRECTION('center_axis',(-2.40370335797945E-16,0.,1.));
#8714=DIRECTION('ref_axis',(-1.,0.,-2.40370335797945E-16));
#8715=DIRECTION('',(-1.,0.,-2.40370335797945E-16));
#8716=DIRECTION('',(0.,-1.,0.));
#8717=DIRECTION('',(-1.,0.,-2.40370335797945E-16));
#8718=DIRECTION('center_axis',(0.866025403784439,0.,0.5));
#8719=DIRECTION('ref_axis',(-0.5,0.,0.866025403784439));
#8720=DIRECTION('',(-0.5,0.,0.866025403784439));
#8721=DIRECTION('',(-0.5,0.,0.866025403784439));
#8722=DIRECTION('center_axis',(0.,-1.,0.));
#8723=DIRECTION('ref_axis',(0.,0.,-1.));
#8724=DIRECTION('center_axis',(0.,1.,0.));
#8725=DIRECTION('ref_axis',(0.,0.,1.));
#8726=DIRECTION('center_axis',(0.,-1.,0.));
#8727=DIRECTION('ref_axis',(1.,0.,0.));
#8728=DIRECTION('center_axis',(0.,-1.,0.));
#8729=DIRECTION('ref_axis',(1.,0.,0.));
#8730=DIRECTION('center_axis',(0.,-1.,0.));
#8731=DIRECTION('ref_axis',(1.,0.,0.));
#8732=DIRECTION('',(0.707106781186548,0.707106781186547,8.65956056235494E-17));
#8733=DIRECTION('center_axis',(0.,-1.,0.));
#8734=DIRECTION('ref_axis',(1.,0.,0.));
#8735=DIRECTION('center_axis',(0.,1.,0.));
#8736=DIRECTION('ref_axis',(1.,0.,0.));
#8737=DIRECTION('',(0.,1.,0.));
#8738=DIRECTION('center_axis',(0.,1.,0.));
#8739=DIRECTION('ref_axis',(1.,0.,0.));
#8740=DIRECTION('center_axis',(0.,-1.,0.));
#8741=DIRECTION('ref_axis',(1.,0.,0.));
#8742=DIRECTION('',(-0.707106781186548,0.707106781186547,-8.65956056235494E-17));
#8743=DIRECTION('center_axis',(0.,-1.,0.));
#8744=DIRECTION('ref_axis',(0.,0.,-1.));
#8745=DIRECTION('axis',(0.,0.,1.));
#8746=DIRECTION('refdir',(1.,0.,0.));
#8747=DIRECTION('axis',(0.,0.,1.));
#8748=DIRECTION('refdir',(1.,0.,0.));
#8749=DIRECTION('center_axis',(0.,0.,1.));
#8750=DIRECTION('ref_axis',(1.,0.,0.));
#8751=DIRECTION('center_axis',(0.,0.,1.));
#8752=DIRECTION('ref_axis',(1.,0.,0.));
#8753=DIRECTION('',(0.,0.,1.));
#8754=DIRECTION('center_axis',(0.,0.,-1.));
#8755=DIRECTION('ref_axis',(1.,0.,0.));
#8756=DIRECTION('center_axis',(0.,0.,1.));
#8757=DIRECTION('ref_axis',(1.,0.,0.));
#8758=DIRECTION('center_axis',(0.,0.,1.));
#8759=DIRECTION('ref_axis',(1.,0.,0.));
#8760=DIRECTION('',(0.,0.,1.));
#8761=DIRECTION('center_axis',(0.,0.,-1.));
#8762=DIRECTION('ref_axis',(1.,0.,0.));
#8763=DIRECTION('center_axis',(0.,0.,1.));
#8764=DIRECTION('ref_axis',(1.,0.,0.));
#8765=DIRECTION('center_axis',(0.,0.,1.));
#8766=DIRECTION('ref_axis',(1.,0.,0.));
#8767=DIRECTION('',(0.,0.,1.));
#8768=DIRECTION('center_axis',(0.,0.,-1.));
#8769=DIRECTION('ref_axis',(1.,0.,0.));
#8770=DIRECTION('center_axis',(0.,0.,1.));
#8771=DIRECTION('ref_axis',(1.,0.,0.));
#8772=DIRECTION('center_axis',(0.,0.,1.));
#8773=DIRECTION('ref_axis',(1.,0.,0.));
#8774=DIRECTION('',(0.,0.,1.));
#8775=DIRECTION('center_axis',(0.,0.,-1.));
#8776=DIRECTION('ref_axis',(1.,0.,0.));
#8777=DIRECTION('center_axis',(0.,0.,1.));
#8778=DIRECTION('ref_axis',(1.,0.,0.));
#8779=DIRECTION('',(0.,-1.,0.));
#8780=DIRECTION('',(-1.,0.,0.));
#8781=DIRECTION('',(0.,1.,0.));
#8782=DIRECTION('',(1.,0.,0.));
#8783=DIRECTION('center_axis',(0.,0.,1.));
#8784=DIRECTION('ref_axis',(1.,0.,0.));
#8785=DIRECTION('center_axis',(0.,1.,0.));
#8786=DIRECTION('ref_axis',(-1.,0.,0.));
#8787=DIRECTION('',(0.,0.,1.));
#8788=DIRECTION('',(-1.,0.,0.));
#8789=DIRECTION('',(0.,0.,1.));
#8790=DIRECTION('center_axis',(1.,0.,0.));
#8791=DIRECTION('ref_axis',(0.,1.,0.));
#8792=DIRECTION('',(0.,1.,0.));
#8793=DIRECTION('',(0.,0.,1.));
#8794=DIRECTION('center_axis',(0.,-1.,0.));
#8795=DIRECTION('ref_axis',(1.,0.,0.));
#8796=DIRECTION('',(1.,0.,0.));
#8797=DIRECTION('',(0.,0.,1.));
#8798=DIRECTION('center_axis',(-1.,0.,0.));
#8799=DIRECTION('ref_axis',(0.,-1.,0.));
#8800=DIRECTION('',(0.,-1.,0.));
#8801=DIRECTION('center_axis',(0.,0.,1.));
#8802=DIRECTION('ref_axis',(1.,0.,0.));
#8803=DIRECTION('center_axis',(0.,0.,1.));
#8804=DIRECTION('ref_axis',(1.,0.,0.));
#8805=DIRECTION('',(0.,0.,-1.));
#8806=DIRECTION('center_axis',(0.,0.,-1.));
#8807=DIRECTION('ref_axis',(1.,0.,0.));
#8808=DIRECTION('center_axis',(0.,0.,1.));
#8809=DIRECTION('ref_axis',(1.,0.,0.));
#8810=DIRECTION('center_axis',(0.,0.,1.));
#8811=DIRECTION('ref_axis',(1.,0.,0.));
#8812=DIRECTION('',(0.,0.,1.));
#8813=DIRECTION('center_axis',(0.,0.,-1.));
#8814=DIRECTION('ref_axis',(1.,0.,0.));
#8815=DIRECTION('center_axis',(0.,0.,1.));
#8816=DIRECTION('ref_axis',(6.12323399573677E-17,1.,0.));
#8817=DIRECTION('',(0.,0.,1.));
#8818=DIRECTION('center_axis',(0.,0.,1.));
#8819=DIRECTION('ref_axis',(1.,0.,0.));
#8820=DIRECTION('',(0.,0.,-1.));
#8821=DIRECTION('center_axis',(0.,0.,1.));
#8822=DIRECTION('ref_axis',(1.,0.,0.));
#8823=DIRECTION('center_axis',(1.,0.,0.));
#8824=DIRECTION('ref_axis',(0.,1.,0.));
#8825=DIRECTION('',(0.,1.,0.));
#8826=DIRECTION('',(0.,0.,1.));
#8827=DIRECTION('',(0.,-1.,0.));
#8828=DIRECTION('center_axis',(0.,0.,1.));
#8829=DIRECTION('ref_axis',(1.,0.,0.));
#8830=DIRECTION('',(0.,-1.,0.));
#8831=DIRECTION('center_axis',(0.,0.,1.));
#8832=DIRECTION('ref_axis',(1.,0.,0.));
#8833=DIRECTION('center_axis',(-1.,0.,0.));
#8834=DIRECTION('ref_axis',(0.,-1.,0.));
#8835=DIRECTION('',(0.,1.,0.));
#8836=DIRECTION('',(0.,0.,-1.));
#8837=DIRECTION('center_axis',(0.,0.,1.));
#8838=DIRECTION('ref_axis',(-1.83697019872103E-16,-1.,0.));
#8839=DIRECTION('center_axis',(0.,0.,1.));
#8840=DIRECTION('ref_axis',(1.,0.,0.));
#8841=DIRECTION('center_axis',(0.,0.,1.));
#8842=DIRECTION('ref_axis',(1.,0.,0.));
#8843=DIRECTION('center_axis',(0.,0.,1.));
#8844=DIRECTION('ref_axis',(1.,0.,0.));
#8845=DIRECTION('center_axis',(0.,0.,1.));
#8846=DIRECTION('ref_axis',(1.,0.,0.));
#8847=DIRECTION('center_axis',(0.,0.,1.));
#8848=DIRECTION('ref_axis',(1.,0.,0.));
#8849=DIRECTION('center_axis',(0.,0.,-1.));
#8850=DIRECTION('ref_axis',(1.,0.,0.));
#8851=DIRECTION('center_axis',(0.,0.,1.));
#8852=DIRECTION('ref_axis',(1.,0.,0.));
#8853=DIRECTION('',(0.,0.,-1.));
#8854=DIRECTION('center_axis',(0.,0.,1.));
#8855=DIRECTION('ref_axis',(1.,0.,0.));
#8856=DIRECTION('',(0.,0.,-1.));
#8857=DIRECTION('center_axis',(0.,0.,1.));
#8858=DIRECTION('ref_axis',(1.,0.,0.));
#8859=DIRECTION('center_axis',(0.,0.,1.));
#8860=DIRECTION('ref_axis',(1.,0.,0.));
#8861=DIRECTION('axis',(0.,0.,1.));
#8862=DIRECTION('refdir',(1.,0.,0.));
#8863=DIRECTION('center_axis',(0.,0.,1.));
#8864=DIRECTION('ref_axis',(1.,0.,0.));
#8865=DIRECTION('center_axis',(0.,0.,-1.));
#8866=DIRECTION('ref_axis',(1.,0.,0.));
#8867=DIRECTION('',(0.,0.,-1.));
#8868=DIRECTION('center_axis',(0.,0.,-1.));
#8869=DIRECTION('ref_axis',(1.,0.,0.));
#8870=DIRECTION('center_axis',(0.,0.,1.));
#8871=DIRECTION('ref_axis',(1.,0.,0.));
#8872=DIRECTION('center_axis',(0.,0.,1.));
#8873=DIRECTION('ref_axis',(1.,0.,0.));
#8874=DIRECTION('',(0.,0.,-1.));
#8875=DIRECTION('center_axis',(0.,0.,1.));
#8876=DIRECTION('ref_axis',(1.,0.,0.));
#8877=DIRECTION('center_axis',(0.,0.,1.));
#8878=DIRECTION('ref_axis',(1.,0.,0.));
#8879=DIRECTION('center_axis',(0.,0.,1.));
#8880=DIRECTION('ref_axis',(1.,0.,0.));
#8881=DIRECTION('axis',(0.,0.,1.));
#8882=DIRECTION('refdir',(1.,0.,0.));
#8883=DIRECTION('center_axis',(1.,0.,0.));
#8884=DIRECTION('ref_axis',(0.,0.,-1.));
#8885=DIRECTION('',(0.,0.,1.));
#8886=DIRECTION('center_axis',(1.,0.,0.));
#8887=DIRECTION('ref_axis',(0.,0.,-1.));
#8888=DIRECTION('center_axis',(1.,0.,0.));
#8889=DIRECTION('ref_axis',(0.,0.,-1.));
#8890=DIRECTION('center_axis',(1.,0.,0.));
#8891=DIRECTION('ref_axis',(0.,0.,-1.));
#8892=DIRECTION('',(1.,0.,0.));
#8893=DIRECTION('center_axis',(1.,0.,0.));
#8894=DIRECTION('ref_axis',(0.,0.,-1.));
#8895=DIRECTION('',(0.,0.,-1.));
#8896=DIRECTION('center_axis',(0.,0.,1.));
#8897=DIRECTION('ref_axis',(1.,0.,0.));
#8898=DIRECTION('center_axis',(0.,0.,-1.));
#8899=DIRECTION('ref_axis',(1.,0.,0.));
#8900=DIRECTION('',(0.,0.,-1.));
#8901=DIRECTION('center_axis',(0.,0.,-1.));
#8902=DIRECTION('ref_axis',(1.,0.,0.));
#8903=DIRECTION('center_axis',(0.,0.,1.));
#8904=DIRECTION('ref_axis',(1.,0.,0.));
#8905=DIRECTION('center_axis',(0.,0.,1.));
#8906=DIRECTION('ref_axis',(1.,0.,0.));
#8907=DIRECTION('',(0.,0.,-1.));
#8908=DIRECTION('center_axis',(0.,0.,1.));
#8909=DIRECTION('ref_axis',(1.,0.,0.));
#8910=DIRECTION('center_axis',(0.,0.,1.));
#8911=DIRECTION('ref_axis',(1.,0.,0.));
#8912=DIRECTION('center_axis',(0.,0.,1.));
#8913=DIRECTION('ref_axis',(1.,0.,0.));
#8914=DIRECTION('axis',(0.,0.,1.));
#8915=DIRECTION('refdir',(1.,0.,0.));
#8916=DIRECTION('center_axis',(0.,0.,1.));
#8917=DIRECTION('ref_axis',(1.,0.,0.));
#8918=DIRECTION('center_axis',(0.,0.,1.));
#8919=DIRECTION('ref_axis',(1.,0.,0.));
#8920=DIRECTION('',(0.,0.,1.));
#8921=DIRECTION('center_axis',(0.,0.,-1.));
#8922=DIRECTION('ref_axis',(1.,0.,0.));
#8923=DIRECTION('center_axis',(0.,0.,1.));
#8924=DIRECTION('ref_axis',(1.,0.,0.));
#8925=DIRECTION('center_axis',(0.,0.,1.));
#8926=DIRECTION('ref_axis',(1.,0.,0.));
#8927=DIRECTION('center_axis',(0.,0.,1.));
#8928=DIRECTION('ref_axis',(1.,0.,0.));
#8929=DIRECTION('',(0.,0.,1.));
#8930=DIRECTION('center_axis',(0.,0.,1.));
#8931=DIRECTION('ref_axis',(1.,0.,0.));
#8932=DIRECTION('center_axis',(0.,0.,1.));
#8933=DIRECTION('ref_axis',(1.,0.,0.));
#8934=DIRECTION('center_axis',(0.,0.,1.));
#8935=DIRECTION('ref_axis',(1.,0.,0.));
#8936=DIRECTION('center_axis',(0.,0.,1.));
#8937=DIRECTION('ref_axis',(1.,0.,0.));
#8938=DIRECTION('center_axis',(0.,0.,1.));
#8939=DIRECTION('ref_axis',(1.,0.,0.));
#8940=DIRECTION('center_axis',(0.,0.,1.));
#8941=DIRECTION('ref_axis',(1.,0.,0.));
#8942=DIRECTION('center_axis',(0.,0.,1.));
#8943=DIRECTION('ref_axis',(1.,0.,0.));
#8944=DIRECTION('center_axis',(0.,0.,-1.));
#8945=DIRECTION('ref_axis',(1.,0.,0.));
#8946=DIRECTION('center_axis',(0.,0.,1.));
#8947=DIRECTION('ref_axis',(1.,0.,0.));
#8948=DIRECTION('',(0.,0.,-1.));
#8949=DIRECTION('center_axis',(0.,0.,1.));
#8950=DIRECTION('ref_axis',(1.,0.,0.));
#8951=DIRECTION('',(0.,0.,-1.));
#8952=DIRECTION('center_axis',(0.,0.,1.));
#8953=DIRECTION('ref_axis',(1.,0.,0.));
#8954=DIRECTION('center_axis',(0.,0.,1.));
#8955=DIRECTION('ref_axis',(1.,0.,0.));
#8956=DIRECTION('center_axis',(0.,0.,1.));
#8957=DIRECTION('ref_axis',(1.,0.,0.));
#8958=DIRECTION('',(0.,0.,-1.));
#8959=DIRECTION('center_axis',(0.,0.,1.));
#8960=DIRECTION('ref_axis',(1.,0.,0.));
#8961=DIRECTION('center_axis',(0.,0.,1.));
#8962=DIRECTION('ref_axis',(1.,0.,0.));
#8963=DIRECTION('axis',(0.,0.,1.));
#8964=DIRECTION('refdir',(1.,0.,0.));
#8965=DIRECTION('center_axis',(0.,0.,1.));
#8966=DIRECTION('ref_axis',(1.,0.,0.));
#8967=DIRECTION('center_axis',(0.,0.,-1.));
#8968=DIRECTION('ref_axis',(1.,0.,0.));
#8969=DIRECTION('',(0.,0.,-1.));
#8970=DIRECTION('center_axis',(0.,0.,-1.));
#8971=DIRECTION('ref_axis',(1.,0.,0.));
#8972=DIRECTION('center_axis',(0.,0.,1.));
#8973=DIRECTION('ref_axis',(1.,0.,0.));
#8974=DIRECTION('center_axis',(0.,0.,1.));
#8975=DIRECTION('ref_axis',(1.,0.,0.));
#8976=DIRECTION('',(0.,0.,-1.));
#8977=DIRECTION('center_axis',(0.,0.,1.));
#8978=DIRECTION('ref_axis',(1.,0.,0.));
#8979=DIRECTION('center_axis',(0.,0.,1.));
#8980=DIRECTION('ref_axis',(1.,0.,0.));
#8981=DIRECTION('center_axis',(0.,0.,1.));
#8982=DIRECTION('ref_axis',(1.,0.,0.));
#8983=DIRECTION('axis',(0.,0.,1.));
#8984=DIRECTION('refdir',(1.,0.,0.));
#8985=DIRECTION('center_axis',(0.,0.,1.));
#8986=DIRECTION('ref_axis',(1.,0.,0.));
#8987=DIRECTION('center_axis',(0.,0.,-1.));
#8988=DIRECTION('ref_axis',(1.,0.,0.));
#8989=DIRECTION('',(0.,0.,-1.));
#8990=DIRECTION('center_axis',(0.,0.,-1.));
#8991=DIRECTION('ref_axis',(1.,0.,0.));
#8992=DIRECTION('center_axis',(0.,0.,1.));
#8993=DIRECTION('ref_axis',(1.,0.,0.));
#8994=DIRECTION('center_axis',(0.,0.,1.));
#8995=DIRECTION('ref_axis',(1.,0.,0.));
#8996=DIRECTION('',(0.,0.,-1.));
#8997=DIRECTION('center_axis',(0.,0.,1.));
#8998=DIRECTION('ref_axis',(1.,0.,0.));
#8999=DIRECTION('center_axis',(0.,0.,1.));
#9000=DIRECTION('ref_axis',(1.,0.,0.));
#9001=DIRECTION('center_axis',(0.,0.,1.));
#9002=DIRECTION('ref_axis',(1.,0.,0.));
#9003=DIRECTION('axis',(0.,0.,1.));
#9004=DIRECTION('refdir',(1.,0.,0.));
#9005=DIRECTION('center_axis',(0.,0.,1.));
#9006=DIRECTION('ref_axis',(1.,0.,0.));
#9007=DIRECTION('center_axis',(0.,0.,-1.));
#9008=DIRECTION('ref_axis',(1.,0.,0.));
#9009=DIRECTION('',(0.,0.,-1.));
#9010=DIRECTION('center_axis',(0.,0.,-1.));
#9011=DIRECTION('ref_axis',(1.,0.,0.));
#9012=DIRECTION('center_axis',(0.,0.,1.));
#9013=DIRECTION('ref_axis',(1.,0.,0.));
#9014=DIRECTION('center_axis',(0.,0.,1.));
#9015=DIRECTION('ref_axis',(1.,0.,0.));
#9016=DIRECTION('',(0.,0.,-1.));
#9017=DIRECTION('center_axis',(0.,0.,1.));
#9018=DIRECTION('ref_axis',(1.,0.,0.));
#9019=DIRECTION('center_axis',(0.,0.,1.));
#9020=DIRECTION('ref_axis',(1.,0.,0.));
#9021=DIRECTION('center_axis',(0.,0.,1.));
#9022=DIRECTION('ref_axis',(1.,0.,0.));
#9023=DIRECTION('axis',(0.,0.,1.));
#9024=DIRECTION('refdir',(1.,0.,0.));
#9025=DIRECTION('center_axis',(0.,0.,1.));
#9026=DIRECTION('ref_axis',(1.,0.,0.));
#9027=DIRECTION('center_axis',(0.,0.,-1.));
#9028=DIRECTION('ref_axis',(1.,0.,0.));
#9029=DIRECTION('',(0.,0.,-1.));
#9030=DIRECTION('center_axis',(0.,0.,-1.));
#9031=DIRECTION('ref_axis',(1.,0.,0.));
#9032=DIRECTION('center_axis',(0.,0.,1.));
#9033=DIRECTION('ref_axis',(1.,0.,0.));
#9034=DIRECTION('center_axis',(0.,0.,1.));
#9035=DIRECTION('ref_axis',(1.,0.,0.));
#9036=DIRECTION('',(0.,0.,-1.));
#9037=DIRECTION('center_axis',(0.,0.,1.));
#9038=DIRECTION('ref_axis',(1.,0.,0.));
#9039=DIRECTION('center_axis',(0.,0.,1.));
#9040=DIRECTION('ref_axis',(1.,0.,0.));
#9041=DIRECTION('center_axis',(0.,0.,1.));
#9042=DIRECTION('ref_axis',(1.,0.,0.));
#9043=DIRECTION('axis',(0.,0.,1.));
#9044=DIRECTION('refdir',(1.,0.,0.));
#9045=DIRECTION('center_axis',(0.,1.,0.));
#9046=DIRECTION('ref_axis',(1.,0.,0.));
#9047=DIRECTION('center_axis',(0.,1.,0.));
#9048=DIRECTION('ref_axis',(1.,0.,0.));
#9049=DIRECTION('center_axis',(0.866025403784439,0.,-0.5));
#9050=DIRECTION('ref_axis',(0.5,0.,0.866025403784439));
#9051=DIRECTION('',(0.5,0.,0.866025403784439));
#9052=DIRECTION('',(0.,-1.,0.));
#9053=DIRECTION('',(0.5,0.,0.866025403784439));
#9054=DIRECTION('',(0.,-1.,0.));
#9055=DIRECTION('center_axis',(1.20185167898973E-16,0.,-1.));
#9056=DIRECTION('ref_axis',(1.,0.,1.20185167898973E-16));
#9057=DIRECTION('',(1.,0.,1.20185167898973E-16));
#9058=DIRECTION('',(0.,-1.,0.));
#9059=DIRECTION('',(1.,0.,1.20185167898973E-16));
#9060=DIRECTION('center_axis',(-0.866025403784439,0.,-0.5));
#9061=DIRECTION('ref_axis',(0.5,0.,-0.866025403784439));
#9062=DIRECTION('',(0.5,0.,-0.866025403784439));
#9063=DIRECTION('',(0.,-1.,0.));
#9064=DIRECTION('',(0.5,0.,-0.866025403784439));
#9065=DIRECTION('center_axis',(-0.866025403784439,0.,0.5));
#9066=DIRECTION('ref_axis',(-0.5,0.,-0.866025403784439));
#9067=DIRECTION('',(-0.5,0.,-0.866025403784439));
#9068=DIRECTION('',(0.,-1.,0.));
#9069=DIRECTION('',(-0.5,0.,-0.866025403784439));
#9070=DIRECTION('center_axis',(-2.40370335797945E-16,0.,1.));
#9071=DIRECTION('ref_axis',(-1.,0.,-2.40370335797945E-16));
#9072=DIRECTION('',(-1.,0.,-2.40370335797945E-16));
#9073=DIRECTION('',(0.,-1.,0.));
#9074=DIRECTION('',(-1.,0.,-2.40370335797945E-16));
#9075=DIRECTION('center_axis',(0.866025403784439,0.,0.5));
#9076=DIRECTION('ref_axis',(-0.5,0.,0.866025403784439));
#9077=DIRECTION('',(-0.5,0.,0.866025403784439));
#9078=DIRECTION('',(-0.5,0.,0.866025403784439));
#9079=DIRECTION('center_axis',(0.,-1.,0.));
#9080=DIRECTION('ref_axis',(0.,0.,-1.));
#9081=DIRECTION('center_axis',(0.,1.,0.));
#9082=DIRECTION('ref_axis',(0.,0.,1.));
#9083=DIRECTION('center_axis',(0.,-1.,0.));
#9084=DIRECTION('ref_axis',(1.,0.,0.));
#9085=DIRECTION('center_axis',(0.,-1.,0.));
#9086=DIRECTION('ref_axis',(1.,0.,0.));
#9087=DIRECTION('center_axis',(0.,-1.,0.));
#9088=DIRECTION('ref_axis',(1.,0.,0.));
#9089=DIRECTION('',(0.707106781186548,0.707106781186547,8.65956056235494E-17));
#9090=DIRECTION('center_axis',(0.,-1.,0.));
#9091=DIRECTION('ref_axis',(1.,0.,0.));
#9092=DIRECTION('',(0.,1.,0.));
#9093=DIRECTION('axis',(0.,0.,1.));
#9094=DIRECTION('refdir',(1.,0.,0.));
#9095=DIRECTION('center_axis',(0.,1.,0.));
#9096=DIRECTION('ref_axis',(0.,0.,1.));
#9097=DIRECTION('center_axis',(0.,-1.,0.));
#9098=DIRECTION('ref_axis',(1.,0.,0.));
#9099=DIRECTION('center_axis',(0.,-1.,0.));
#9100=DIRECTION('ref_axis',(1.,0.,0.));
#9101=DIRECTION('center_axis',(0.,-1.,0.));
#9102=DIRECTION('ref_axis',(1.,0.,0.));
#9103=DIRECTION('',(0.707106781186547,0.707106781186548,8.65956056235493E-17));
#9104=DIRECTION('center_axis',(0.,-1.,0.));
#9105=DIRECTION('ref_axis',(1.,0.,0.));
#9106=DIRECTION('center_axis',(0.,-1.,0.));
#9107=DIRECTION('ref_axis',(1.,0.,0.));
#9108=DIRECTION('',(0.,1.,0.));
#9109=DIRECTION('center_axis',(0.,1.,0.));
#9110=DIRECTION('ref_axis',(1.,0.,0.));
#9111=DIRECTION('center_axis',(0.,-1.,0.));
#9112=DIRECTION('ref_axis',(1.,0.,0.));
#9113=DIRECTION('',(-0.707106781186547,0.707106781186548,-8.65956056235493E-17));
#9114=DIRECTION('center_axis',(0.,-1.,0.));
#9115=DIRECTION('ref_axis',(0.,0.,-1.));
#9116=DIRECTION('center_axis',(0.,-1.,0.));
#9117=DIRECTION('ref_axis',(1.,0.,0.));
#9118=DIRECTION('center_axis',(0.,1.,0.));
#9119=DIRECTION('ref_axis',(1.,0.,0.));
#9120=DIRECTION('center_axis',(0.,1.,0.));
#9121=DIRECTION('ref_axis',(1.,0.,0.));
#9122=DIRECTION('',(-0.447213595499958,0.894427190999916,-5.47678698264203E-17));
#9123=DIRECTION('center_axis',(0.,-1.,0.));
#9124=DIRECTION('ref_axis',(1.,0.,0.));
#9125=DIRECTION('center_axis',(0.,1.,0.));
#9126=DIRECTION('ref_axis',(1.,0.,0.));
#9127=DIRECTION('',(0.,1.,0.));
#9128=DIRECTION('center_axis',(0.,1.,0.));
#9129=DIRECTION('ref_axis',(1.,0.,0.));
#9130=DIRECTION('center_axis',(0.,-1.,0.));
#9131=DIRECTION('ref_axis',(1.,0.,0.));
#9132=DIRECTION('',(-0.707106781186547,0.707106781186548,-8.65956056235493E-17));
#9133=DIRECTION('center_axis',(0.,-1.,0.));
#9134=DIRECTION('ref_axis',(0.,0.,-1.));
#9135=DIRECTION('center_axis',(0.866025403784439,0.,-0.5));
#9136=DIRECTION('ref_axis',(0.5,0.,0.866025403784439));
#9137=DIRECTION('',(-0.5,0.,-0.866025403784439));
#9138=DIRECTION('',(0.,-1.,0.));
#9139=DIRECTION('',(0.5,0.,0.866025403784439));
#9140=DIRECTION('',(0.,-1.,0.));
#9141=DIRECTION('center_axis',(1.60246890531964E-16,0.,-1.));
#9142=DIRECTION('ref_axis',(1.,0.,1.60246890531964E-16));
#9143=DIRECTION('',(-1.,0.,-1.60246890531964E-16));
#9144=DIRECTION('',(0.,-1.,0.));
#9145=DIRECTION('',(1.,0.,1.60246890531964E-16));
#9146=DIRECTION('center_axis',(-0.866025403784439,0.,-0.5));
#9147=DIRECTION('ref_axis',(0.5,0.,-0.866025403784439));
#9148=DIRECTION('',(-0.5,0.,0.866025403784439));
#9149=DIRECTION('',(0.,-1.,0.));
#9150=DIRECTION('',(0.5,0.,-0.866025403784439));
#9151=DIRECTION('center_axis',(-0.866025403784439,0.,0.5));
#9152=DIRECTION('ref_axis',(-0.5,0.,-0.866025403784439));
#9153=DIRECTION('',(0.5,0.,0.866025403784439));
#9154=DIRECTION('',(0.,-1.,0.));
#9155=DIRECTION('',(-0.5,0.,-0.866025403784439));
#9156=DIRECTION('center_axis',(-1.60246890531964E-16,0.,1.));
#9157=DIRECTION('ref_axis',(-1.,0.,-1.60246890531964E-16));
#9158=DIRECTION('',(1.,0.,1.60246890531964E-16));
#9159=DIRECTION('',(0.,-1.,0.));
#9160=DIRECTION('',(-1.,0.,-1.60246890531964E-16));
#9161=DIRECTION('center_axis',(0.866025403784439,0.,0.5));
#9162=DIRECTION('ref_axis',(-0.5,0.,0.866025403784439));
#9163=DIRECTION('',(0.5,0.,-0.866025403784439));
#9164=DIRECTION('',(-0.5,0.,0.866025403784439));
#9165=DIRECTION('center_axis',(0.,1.,0.));
#9166=DIRECTION('ref_axis',(1.,0.,0.));
#9167=DIRECTION('center_axis',(0.,-1.,0.));
#9168=DIRECTION('ref_axis',(0.,0.,-1.));
#9169=DIRECTION('axis',(0.,0.,1.));
#9170=DIRECTION('refdir',(1.,0.,0.));
#9171=DIRECTION('center_axis',(0.866025403784439,0.,-0.5));
#9172=DIRECTION('ref_axis',(0.5,0.,0.866025403784439));
#9173=DIRECTION('',(-0.5,0.,-0.866025403784439));
#9174=DIRECTION('',(0.,-1.,0.));
#9175=DIRECTION('',(0.5,0.,0.866025403784439));
#9176=DIRECTION('',(0.,-1.,0.));
#9177=DIRECTION('center_axis',(1.60246890531964E-16,0.,-1.));
#9178=DIRECTION('ref_axis',(1.,0.,1.60246890531964E-16));
#9179=DIRECTION('',(-1.,0.,-1.60246890531964E-16));
#9180=DIRECTION('',(0.,-1.,0.));
#9181=DIRECTION('',(1.,0.,1.60246890531964E-16));
#9182=DIRECTION('center_axis',(-0.866025403784439,0.,-0.5));
#9183=DIRECTION('ref_axis',(0.5,0.,-0.866025403784439));
#9184=DIRECTION('',(-0.5,0.,0.866025403784439));
#9185=DIRECTION('',(0.,-1.,0.));
#9186=DIRECTION('',(0.5,0.,-0.866025403784439));
#9187=DIRECTION('center_axis',(-0.866025403784439,0.,0.5));
#9188=DIRECTION('ref_axis',(-0.5,0.,-0.866025403784439));
#9189=DIRECTION('',(0.5,0.,0.866025403784439));
#9190=DIRECTION('',(0.,-1.,0.));
#9191=DIRECTION('',(-0.5,0.,-0.866025403784439));
#9192=DIRECTION('center_axis',(-1.60246890531964E-16,0.,1.));
#9193=DIRECTION('ref_axis',(-1.,0.,-1.60246890531964E-16));
#9194=DIRECTION('',(1.,0.,1.60246890531964E-16));
#9195=DIRECTION('',(0.,-1.,0.));
#9196=DIRECTION('',(-1.,0.,-1.60246890531964E-16));
#9197=DIRECTION('center_axis',(0.866025403784439,0.,0.5));
#9198=DIRECTION('ref_axis',(-0.5,0.,0.866025403784439));
#9199=DIRECTION('',(0.5,0.,-0.866025403784439));
#9200=DIRECTION('',(-0.5,0.,0.866025403784439));
#9201=DIRECTION('center_axis',(0.,1.,0.));
#9202=DIRECTION('ref_axis',(1.,0.,0.));
#9203=DIRECTION('center_axis',(0.,-1.,0.));
#9204=DIRECTION('ref_axis',(0.,0.,-1.));
#9205=DIRECTION('center_axis',(0.,1.,0.));
#9206=DIRECTION('ref_axis',(1.,0.,0.));
#9207=DIRECTION('center_axis',(0.,1.,0.));
#9208=DIRECTION('ref_axis',(1.,0.,0.));
#9209=DIRECTION('center_axis',(0.,1.,0.));
#9210=DIRECTION('ref_axis',(0.,0.,1.));
#9211=DIRECTION('center_axis',(0.,-1.,0.));
#9212=DIRECTION('ref_axis',(1.,0.,0.));
#9213=DIRECTION('center_axis',(0.,-1.,0.));
#9214=DIRECTION('ref_axis',(1.,0.,0.));
#9215=DIRECTION('center_axis',(0.,-1.,0.));
#9216=DIRECTION('ref_axis',(1.,0.,0.));
#9217=DIRECTION('',(0.707106781186547,0.707106781186548,8.65956056235493E-17));
#9218=DIRECTION('center_axis',(0.,-1.,0.));
#9219=DIRECTION('ref_axis',(1.,0.,0.));
#9220=DIRECTION('center_axis',(0.,-1.,0.));
#9221=DIRECTION('ref_axis',(1.,0.,0.));
#9222=DIRECTION('',(0.,1.,0.));
#9223=DIRECTION('center_axis',(0.,1.,0.));
#9224=DIRECTION('ref_axis',(1.,0.,0.));
#9225=DIRECTION('center_axis',(0.,-1.,0.));
#9226=DIRECTION('ref_axis',(1.,0.,0.));
#9227=DIRECTION('',(-0.707106781186547,0.707106781186548,-8.65956056235493E-17));
#9228=DIRECTION('center_axis',(0.,-1.,0.));
#9229=DIRECTION('ref_axis',(0.,0.,-1.));
#9230=DIRECTION('center_axis',(0.,-1.,0.));
#9231=DIRECTION('ref_axis',(1.,0.,0.));
#9232=DIRECTION('center_axis',(0.,1.,0.));
#9233=DIRECTION('ref_axis',(1.,0.,0.));
#9234=DIRECTION('center_axis',(0.,1.,0.));
#9235=DIRECTION('ref_axis',(1.,0.,0.));
#9236=DIRECTION('',(-0.447213595499958,0.894427190999916,-5.47678698264203E-17));
#9237=DIRECTION('center_axis',(0.,-1.,0.));
#9238=DIRECTION('ref_axis',(1.,0.,0.));
#9239=DIRECTION('',(0.,1.,0.));
#9240=DIRECTION('',(0.,0.,1.));
#9241=DIRECTION('',(1.,0.,0.));
#9242=DIRECTION('',(0.,0.,1.));
#9243=DIRECTION('',(1.,0.,0.));
#9244=DIRECTION('',(0.,0.,1.));
#9245=DIRECTION('',(1.,0.,0.));
#9246=DIRECTION('',(0.,0.,1.));
#9247=DIRECTION('',(1.,0.,0.));
#9248=DIRECTION('',(0.,0.,1.));
#9249=DIRECTION('',(1.,0.,0.));
#9250=DIRECTION('',(0.,0.,1.));
#9251=DIRECTION('',(1.,0.,0.));
#9252=DIRECTION('',(0.,0.,1.));
#9253=DIRECTION('',(1.,0.,0.));
#9254=DIRECTION('',(0.,0.,1.));
#9255=DIRECTION('',(1.,0.,0.));
#9256=DIRECTION('',(0.,-1.,2.22044604925031E-16));
#9257=DIRECTION('',(1.,0.,0.));
#9258=DIRECTION('',(0.,-1.,2.22044604925031E-16));
#9259=DIRECTION('',(1.,0.,0.));
#9260=DIRECTION('',(0.,-1.,2.22044604925031E-16));
#9261=DIRECTION('',(1.,0.,0.));
#9262=DIRECTION('',(0.,-1.,2.22044604925031E-16));
#9263=DIRECTION('',(1.,0.,0.));
#9264=DIRECTION('',(0.,-1.,2.22044604925031E-16));
#9265=DIRECTION('',(1.,0.,0.));
#9266=DIRECTION('',(0.,-1.,2.22044604925031E-16));
#9267=DIRECTION('',(1.,0.,0.));
#9268=DIRECTION('',(0.,-1.,2.22044604925031E-16));
#9269=DIRECTION('',(1.,0.,0.));
#9270=DIRECTION('',(0.,-1.,2.22044604925031E-16));
#9271=DIRECTION('',(1.,0.,0.));
#9272=DIRECTION('',(0.,-1.,2.22044604925031E-16));
#9273=DIRECTION('',(1.,0.,0.));
#9274=DIRECTION('',(0.,-1.,2.22044604925031E-16));
#9275=DIRECTION('',(1.,0.,0.));
#9276=DIRECTION('',(0.,-1.,2.22044604925031E-16));
#9277=DIRECTION('',(1.,0.,0.));
#9278=DIRECTION('',(0.,-1.,2.22044604925031E-16));
#9279=DIRECTION('',(1.,0.,0.));
#9280=DIRECTION('',(0.,-1.,2.22044604925031E-16));
#9281=DIRECTION('',(1.,0.,0.));
#9282=DIRECTION('',(0.,-1.,2.22044604925031E-16));
#9283=DIRECTION('',(1.,0.,0.));
#9284=DIRECTION('',(0.,-1.,2.22044604925031E-16));
#9285=DIRECTION('',(1.,0.,0.));
#9286=DIRECTION('',(0.,-1.,2.22044604925031E-16));
#9287=DIRECTION('',(1.,0.,0.));
#9288=DIRECTION('',(0.,-1.,2.22044604925031E-16));
#9289=DIRECTION('',(1.,0.,0.));
#9290=DIRECTION('',(0.,-1.,2.22044604925031E-16));
#9291=DIRECTION('',(1.,0.,0.));
#9292=DIRECTION('',(0.,-1.,2.22044604925031E-16));
#9293=DIRECTION('',(1.,0.,0.));
#9294=DIRECTION('',(0.,0.,1.));
#9295=DIRECTION('',(1.,0.,0.));
#9296=DIRECTION('',(0.,0.,1.));
#9297=DIRECTION('',(1.,0.,0.));
#9298=DIRECTION('',(0.,0.,1.));
#9299=DIRECTION('',(1.,0.,0.));
#9300=DIRECTION('',(0.,0.,1.));
#9301=DIRECTION('',(1.,0.,0.));
#9302=DIRECTION('',(0.,0.,1.));
#9303=DIRECTION('',(1.,0.,0.));
#9304=DIRECTION('',(0.,0.,1.));
#9305=DIRECTION('',(1.,0.,0.));
#9306=DIRECTION('',(0.,0.,1.));
#9307=DIRECTION('',(1.,0.,0.));
#9308=DIRECTION('',(0.,0.,1.));
#9309=DIRECTION('',(1.,0.,0.));
#9310=DIRECTION('',(0.,0.,1.));
#9311=DIRECTION('',(1.,0.,0.));
#9312=DIRECTION('',(0.,0.,1.));
#9313=DIRECTION('',(1.,0.,0.));
#9314=DIRECTION('',(0.,0.,1.));
#9315=DIRECTION('',(1.,0.,0.));
#9316=DIRECTION('',(0.,0.,1.));
#9317=DIRECTION('',(2.22044604925031E-16,-1.,0.));
#9318=DIRECTION('',(0.,0.,1.));
#9319=DIRECTION('',(2.22044604925031E-16,-1.,0.));
#9320=DIRECTION('',(0.,-1.,2.22044604925031E-16));
#9321=DIRECTION('',(1.,0.,0.));
#9322=DIRECTION('',(0.,1.,2.22044604925031E-16));
#9323=DIRECTION('',(1.,0.,0.));
#9324=DIRECTION('',(0.,-1.,2.22044604925031E-16));
#9325=DIRECTION('',(1.,0.,0.));
#9326=DIRECTION('',(0.,0.,1.));
#9327=DIRECTION('',(1.,0.,0.));
#9328=DIRECTION('',(0.,0.,1.));
#9329=DIRECTION('',(1.,0.,0.));
#9330=DIRECTION('',(0.,0.,1.));
#9331=DIRECTION('',(1.,0.,0.));
#9332=DIRECTION('',(0.,0.,1.));
#9333=DIRECTION('',(1.,0.,0.));
#9334=DIRECTION('',(0.,0.,1.));
#9335=DIRECTION('',(1.,0.,0.));
#9336=DIRECTION('',(0.,0.,1.));
#9337=DIRECTION('',(1.,0.,0.));
#9338=DIRECTION('',(0.,0.,1.));
#9339=DIRECTION('',(1.,0.,0.));
#9340=DIRECTION('',(0.,0.,1.));
#9341=DIRECTION('',(1.,0.,0.));
#9342=DIRECTION('',(0.,0.,1.));
#9343=DIRECTION('',(2.22044604925031E-16,-1.,0.));
#9344=DIRECTION('',(0.,1.,2.22044604925031E-16));
#9345=DIRECTION('',(1.,0.,0.));
#9346=DIRECTION('',(0.,-1.,2.22044604925031E-16));
#9347=DIRECTION('',(1.,0.,0.));
#9348=DIRECTION('axis',(0.,0.,1.));
#9349=DIRECTION('refdir',(1.,0.,0.));
#9350=DIRECTION('axis',(0.,0.,1.));
#9351=DIRECTION('refdir',(1.,0.,0.));
#9352=DIRECTION('center_axis',(0.,0.,1.));
#9353=DIRECTION('ref_axis',(1.,0.,0.));
#9354=DIRECTION('center_axis',(0.,0.,1.));
#9355=DIRECTION('ref_axis',(1.,0.,0.));
#9356=DIRECTION('',(0.,0.,1.));
#9357=DIRECTION('center_axis',(0.,0.,-1.));
#9358=DIRECTION('ref_axis',(1.,0.,0.));
#9359=DIRECTION('center_axis',(0.,0.,1.));
#9360=DIRECTION('ref_axis',(1.,0.,0.));
#9361=DIRECTION('center_axis',(0.,0.,1.));
#9362=DIRECTION('ref_axis',(1.,0.,0.));
#9363=DIRECTION('',(0.,0.,1.));
#9364=DIRECTION('center_axis',(0.,0.,-1.));
#9365=DIRECTION('ref_axis',(1.,0.,0.));
#9366=DIRECTION('center_axis',(0.,0.,1.));
#9367=DIRECTION('ref_axis',(1.,0.,0.));
#9368=DIRECTION('',(0.,0.,-1.));
#9369=DIRECTION('center_axis',(0.,0.,1.));
#9370=DIRECTION('ref_axis',(1.,0.,0.));
#9371=DIRECTION('',(0.,0.,1.));
#9372=DIRECTION('center_axis',(0.,0.,1.));
#9373=DIRECTION('ref_axis',(1.,0.,0.));
#9374=DIRECTION('center_axis',(-0.162294462269189,0.986742371400334,0.));
#9375=DIRECTION('ref_axis',(-0.986742371400334,-0.162294462269189,0.));
#9376=DIRECTION('',(0.986742371400334,0.162294462269189,0.));
#9377=DIRECTION('',(0.,0.,-1.));
#9378=DIRECTION('',(-0.986742371400334,-0.162294462269189,0.));
#9379=DIRECTION('center_axis',(0.,0.,1.));
#9380=DIRECTION('ref_axis',(1.,0.,0.));
#9381=DIRECTION('',(-0.986742371400334,-0.162294462269189,0.));
#9382=DIRECTION('center_axis',(0.,0.,1.));
#9383=DIRECTION('ref_axis',(1.,0.,0.));
#9384=DIRECTION('center_axis',(0.162294462269189,-0.986742371400334,0.));
#9385=DIRECTION('ref_axis',(0.986742371400334,0.162294462269189,0.));
#9386=DIRECTION('',(0.986742371400334,0.162294462269189,0.));
#9387=DIRECTION('',(0.,0.,1.));
#9388=DIRECTION('center_axis',(0.,0.,1.));
#9389=DIRECTION('ref_axis',(-0.986742371400334,-0.162294462269189,0.));
#9390=DIRECTION('center_axis',(0.,0.,1.));
#9391=DIRECTION('ref_axis',(1.,0.,0.));
#9392=DIRECTION('center_axis',(0.,0.,1.));
#9393=DIRECTION('ref_axis',(1.,0.,0.));
#9394=DIRECTION('axis',(0.,0.,1.));
#9395=DIRECTION('refdir',(1.,0.,0.));
#9396=DIRECTION('center_axis',(0.,0.,1.));
#9397=DIRECTION('ref_axis',(1.,0.,0.));
#9398=DIRECTION('center_axis',(0.,0.,-1.));
#9399=DIRECTION('ref_axis',(1.,0.,0.));
#9400=DIRECTION('',(0.,0.,-1.));
#9401=DIRECTION('center_axis',(0.,0.,-1.));
#9402=DIRECTION('ref_axis',(1.,0.,0.));
#9403=DIRECTION('center_axis',(0.,0.,1.));
#9404=DIRECTION('ref_axis',(1.,0.,0.));
#9405=DIRECTION('center_axis',(0.,0.,1.));
#9406=DIRECTION('ref_axis',(1.,0.,0.));
#9407=DIRECTION('',(0.,0.,-1.));
#9408=DIRECTION('center_axis',(0.,0.,1.));
#9409=DIRECTION('ref_axis',(1.,0.,0.));
#9410=DIRECTION('center_axis',(0.,0.,1.));
#9411=DIRECTION('ref_axis',(1.,0.,0.));
#9412=DIRECTION('center_axis',(0.,0.,1.));
#9413=DIRECTION('ref_axis',(1.,0.,0.));
#9414=DIRECTION('axis',(0.,0.,1.));
#9415=DIRECTION('refdir',(1.,0.,0.));
#9416=DIRECTION('center_axis',(0.,0.,1.));
#9417=DIRECTION('ref_axis',(1.,0.,0.));
#9418=DIRECTION('center_axis',(0.,0.,-1.));
#9419=DIRECTION('ref_axis',(1.,0.,0.));
#9420=DIRECTION('',(0.,0.,-1.));
#9421=DIRECTION('center_axis',(0.,0.,-1.));
#9422=DIRECTION('ref_axis',(1.,0.,0.));
#9423=DIRECTION('center_axis',(0.,0.,1.));
#9424=DIRECTION('ref_axis',(1.,0.,0.));
#9425=DIRECTION('center_axis',(0.,0.,1.));
#9426=DIRECTION('ref_axis',(1.,0.,0.));
#9427=DIRECTION('',(0.,0.,-1.));
#9428=DIRECTION('center_axis',(0.,0.,1.));
#9429=DIRECTION('ref_axis',(1.,0.,0.));
#9430=DIRECTION('center_axis',(0.,0.,1.));
#9431=DIRECTION('ref_axis',(1.,0.,0.));
#9432=DIRECTION('center_axis',(0.,0.,1.));
#9433=DIRECTION('ref_axis',(1.,0.,0.));
#9434=DIRECTION('',(0.,0.,1.));
#9435=DIRECTION('',(1.,0.,0.));
#9436=DIRECTION('',(0.,0.,1.));
#9437=DIRECTION('',(1.,0.,0.));
#9438=DIRECTION('',(0.,0.,1.));
#9439=DIRECTION('',(1.,0.,0.));
#9440=DIRECTION('',(0.,0.,1.));
#9441=DIRECTION('',(1.,0.,0.));
#9442=DIRECTION('',(0.,0.,1.));
#9443=DIRECTION('',(1.,0.,0.));
#9444=DIRECTION('',(0.,0.,1.));
#9445=DIRECTION('',(1.,0.,0.));
#9446=DIRECTION('',(0.,0.,1.));
#9447=DIRECTION('',(1.,0.,0.));
#9448=CARTESIAN_POINT('',(0.,0.,0.));
#9449=CARTESIAN_POINT('',(0.,0.,0.));
#9450=CARTESIAN_POINT('',(0.,0.,0.));
#9451=CARTESIAN_POINT('Origin',(6.23223304703363,-1.76776695296637,-0.1));
#9452=CARTESIAN_POINT('',(6.02223304703363,-1.76776695296637,0.));
#9453=CARTESIAN_POINT('Origin',(6.23223304703363,-1.76776695296637,0.));
#9454=CARTESIAN_POINT('',(6.02223304703363,-1.76776695296637,1.));
#9455=CARTESIAN_POINT('',(6.02223304703363,-1.76776695296637,-0.1));
#9456=CARTESIAN_POINT('Origin',(6.23223304703363,-1.76776695296637,1.));
#9457=CARTESIAN_POINT('Origin',(6.23223304703363,1.76776695296637,-0.1));
#9458=CARTESIAN_POINT('',(6.02223304703363,1.76776695296637,0.));
#9459=CARTESIAN_POINT('Origin',(6.23223304703363,1.76776695296637,0.));
#9460=CARTESIAN_POINT('',(6.02223304703363,1.76776695296637,1.));
#9461=CARTESIAN_POINT('',(6.02223304703363,1.76776695296637,-0.1));
#9462=CARTESIAN_POINT('Origin',(6.23223304703363,1.76776695296637,1.));
#9463=CARTESIAN_POINT('Origin',(9.76776695296637,1.76776695296637,-0.1));
#9464=CARTESIAN_POINT('',(9.55776695296637,1.76776695296637,0.));
#9465=CARTESIAN_POINT('Origin',(9.76776695296637,1.76776695296637,0.));
#9466=CARTESIAN_POINT('',(9.55776695296637,1.76776695296637,1.));
#9467=CARTESIAN_POINT('',(9.55776695296637,1.76776695296637,-0.1));
#9468=CARTESIAN_POINT('Origin',(9.76776695296637,1.76776695296637,1.));
#9469=CARTESIAN_POINT('Origin',(9.76776695296637,-1.76776695296637,-0.1));
#9470=CARTESIAN_POINT('',(9.55776695296637,-1.76776695296637,0.));
#9471=CARTESIAN_POINT('Origin',(9.76776695296637,-1.76776695296637,0.));
#9472=CARTESIAN_POINT('',(9.55776695296637,-1.76776695296637,1.));
#9473=CARTESIAN_POINT('',(9.55776695296637,-1.76776695296637,-0.1));
#9474=CARTESIAN_POINT('Origin',(9.76776695296637,-1.76776695296637,1.));
#9475=CARTESIAN_POINT('Origin',(-1.76776695296637,-1.76776695296637,-0.1));
#9476=CARTESIAN_POINT('',(-1.97776695296637,-1.76776695296637,0.));
#9477=CARTESIAN_POINT('Origin',(-1.76776695296637,-1.76776695296637,0.));
#9478=CARTESIAN_POINT('',(-1.97776695296637,-1.76776695296637,1.));
#9479=CARTESIAN_POINT('',(-1.97776695296637,-1.76776695296637,-0.1));
#9480=CARTESIAN_POINT('Origin',(-1.76776695296637,-1.76776695296637,1.));
#9481=CARTESIAN_POINT('Origin',(-1.76776695296637,1.76776695296637,-0.1));
#9482=CARTESIAN_POINT('',(-1.97776695296637,1.76776695296637,0.));
#9483=CARTESIAN_POINT('Origin',(-1.76776695296637,1.76776695296637,0.));
#9484=CARTESIAN_POINT('',(-1.97776695296637,1.76776695296637,1.));
#9485=CARTESIAN_POINT('',(-1.97776695296637,1.76776695296637,-0.1));
#9486=CARTESIAN_POINT('Origin',(-1.76776695296637,1.76776695296637,1.));
#9487=CARTESIAN_POINT('Origin',(1.76776695296637,1.76776695296637,-0.1));
#9488=CARTESIAN_POINT('',(1.55776695296637,1.76776695296637,0.));
#9489=CARTESIAN_POINT('Origin',(1.76776695296637,1.76776695296637,0.));
#9490=CARTESIAN_POINT('',(1.55776695296637,1.76776695296637,1.));
#9491=CARTESIAN_POINT('',(1.55776695296637,1.76776695296637,-0.1));
#9492=CARTESIAN_POINT('Origin',(1.76776695296637,1.76776695296637,1.));
#9493=CARTESIAN_POINT('Origin',(1.76776695296637,-1.76776695296637,-0.1));
#9494=CARTESIAN_POINT('',(1.55776695296637,-1.76776695296637,0.));
#9495=CARTESIAN_POINT('Origin',(1.76776695296637,-1.76776695296637,0.));
#9496=CARTESIAN_POINT('',(1.55776695296637,-1.76776695296637,1.));
#9497=CARTESIAN_POINT('',(1.55776695296637,-1.76776695296637,-0.1));
#9498=CARTESIAN_POINT('Origin',(1.76776695296637,-1.76776695296637,1.));
#9499=CARTESIAN_POINT('Origin',(12.,6.5,0.));
#9500=CARTESIAN_POINT('',(12.,6.5,0.));
#9501=CARTESIAN_POINT('',(-4.,6.5,0.));
#9502=CARTESIAN_POINT('',(12.,6.5,0.));
#9503=CARTESIAN_POINT('',(-4.,6.5,1.));
#9504=CARTESIAN_POINT('',(-4.,6.5,0.));
#9505=CARTESIAN_POINT('',(12.,6.5,1.));
#9506=CARTESIAN_POINT('',(12.,6.5,1.));
#9507=CARTESIAN_POINT('',(12.,6.5,0.));
#9508=CARTESIAN_POINT('Origin',(12.,-4.,0.));
#9509=CARTESIAN_POINT('',(12.,-4.,0.));
#9510=CARTESIAN_POINT('',(12.,-4.,0.));
#9511=CARTESIAN_POINT('',(12.,-4.,1.));
#9512=CARTESIAN_POINT('',(12.,-4.,1.));
#9513=CARTESIAN_POINT('',(12.,-4.,0.));
#9514=CARTESIAN_POINT('Origin',(-4.,-4.,0.));
#9515=CARTESIAN_POINT('',(-4.,-4.,0.));
#9516=CARTESIAN_POINT('',(-4.,-4.,0.));
#9517=CARTESIAN_POINT('',(-4.,-4.,1.));
#9518=CARTESIAN_POINT('',(-4.,-4.,1.));
#9519=CARTESIAN_POINT('',(-4.,-4.,0.));
#9520=CARTESIAN_POINT('Origin',(-4.,6.5,0.));
#9521=CARTESIAN_POINT('',(-4.,6.5,0.));
#9522=CARTESIAN_POINT('',(-4.,6.5,1.));
#9523=CARTESIAN_POINT('Origin',(4.,1.25,1.));
#9524=CARTESIAN_POINT('Origin',(4.,1.25,0.));
#9525=CARTESIAN_POINT('',(0.,0.,0.));
#9526=CARTESIAN_POINT('Origin',(12.,-3.,-0.5));
#9527=CARTESIAN_POINT('',(12.,-3.,-0.5));
#9528=CARTESIAN_POINT('',(-4.,-3.,-0.5));
#9529=CARTESIAN_POINT('',(12.,-3.,-0.5));
#9530=CARTESIAN_POINT('',(-4.,-3.,0.));
#9531=CARTESIAN_POINT('',(-4.,-3.,-0.5));
#9532=CARTESIAN_POINT('',(12.,-3.,0.));
#9533=CARTESIAN_POINT('',(12.,-3.,0.));
#9534=CARTESIAN_POINT('',(12.,-3.,-0.5));
#9535=CARTESIAN_POINT('Origin',(12.,-4.,-0.5));
#9536=CARTESIAN_POINT('',(12.,-4.,-0.5));
#9537=CARTESIAN_POINT('',(12.,-4.,-0.5));
#9538=CARTESIAN_POINT('',(12.,-4.,0.));
#9539=CARTESIAN_POINT('',(12.,-4.,0.));
#9540=CARTESIAN_POINT('',(12.,-4.,-0.5));
#9541=CARTESIAN_POINT('Origin',(-4.,-4.,-0.5));
#9542=CARTESIAN_POINT('',(-4.,-4.,-0.5));
#9543=CARTESIAN_POINT('',(-4.,-4.,-0.5));
#9544=CARTESIAN_POINT('',(-4.,-4.,0.));
#9545=CARTESIAN_POINT('',(-4.,-4.,0.));
#9546=CARTESIAN_POINT('',(-4.,-4.,-0.5));
#9547=CARTESIAN_POINT('Origin',(-4.,-3.,-0.5));
#9548=CARTESIAN_POINT('',(-4.,-3.,-0.5));
#9549=CARTESIAN_POINT('',(-4.,-3.,0.));
#9550=CARTESIAN_POINT('Origin',(4.,-3.5,0.));
#9551=CARTESIAN_POINT('Origin',(4.,-3.5,-0.5));
#9552=CARTESIAN_POINT('',(0.,0.,0.));
#9553=CARTESIAN_POINT('Origin',(12.,6.5,-0.5));
#9554=CARTESIAN_POINT('',(12.,6.5,-0.5));
#9555=CARTESIAN_POINT('',(-4.,6.5,-0.5));
#9556=CARTESIAN_POINT('',(12.,6.5,-0.5));
#9557=CARTESIAN_POINT('',(-4.,6.5,0.));
#9558=CARTESIAN_POINT('',(-4.,6.5,-0.5));
#9559=CARTESIAN_POINT('',(12.,6.5,0.));
#9560=CARTESIAN_POINT('',(12.,6.5,0.));
#9561=CARTESIAN_POINT('',(12.,6.5,-0.5));
#9562=CARTESIAN_POINT('Origin',(12.,5.5,-0.5));
#9563=CARTESIAN_POINT('',(12.,5.5,-0.5));
#9564=CARTESIAN_POINT('',(12.,5.5,-0.5));
#9565=CARTESIAN_POINT('',(12.,5.5,0.));
#9566=CARTESIAN_POINT('',(12.,5.5,0.));
#9567=CARTESIAN_POINT('',(12.,5.5,-0.5));
#9568=CARTESIAN_POINT('Origin',(-4.,5.5,-0.5));
#9569=CARTESIAN_POINT('',(-4.,5.5,-0.5));
#9570=CARTESIAN_POINT('',(-4.,5.5,-0.5));
#9571=CARTESIAN_POINT('',(-4.,5.5,0.));
#9572=CARTESIAN_POINT('',(-4.,5.5,0.));
#9573=CARTESIAN_POINT('',(-4.,5.5,-0.5));
#9574=CARTESIAN_POINT('Origin',(-4.,6.5,-0.5));
#9575=CARTESIAN_POINT('',(-4.,6.5,-0.5));
#9576=CARTESIAN_POINT('',(-4.,6.5,0.));
#9577=CARTESIAN_POINT('Origin',(4.,6.,0.));
#9578=CARTESIAN_POINT('Origin',(4.,6.,-0.5));
#9579=CARTESIAN_POINT('',(0.,0.,0.));
#9580=CARTESIAN_POINT('Origin',(-1.76776695296637,-1.76776695296637,2.4));
#9581=CARTESIAN_POINT('',(-1.8139637388702,-1.24480341984751,2.4));
#9582=CARTESIAN_POINT('',(-1.24480341984751,-1.81396373887019,2.4));
#9583=CARTESIAN_POINT('Origin',(0.,0.,2.4));
#9584=CARTESIAN_POINT('Origin',(-1.76776695296637,-1.76776695296637,2.4));
#9585=CARTESIAN_POINT('Origin',(-1.76776695296637,-1.76776695296637,1.8));
#9586=CARTESIAN_POINT('',(-1.8139637388702,-1.24480341984751,1.8));
#9587=CARTESIAN_POINT('',(-1.8139637388702,-1.24480341984751,1.8));
#9588=CARTESIAN_POINT('',(-1.24480341984751,-1.81396373887019,1.8));
#9589=CARTESIAN_POINT('Origin',(-1.76776695296637,-1.76776695296637,1.8));
#9590=CARTESIAN_POINT('',(-1.24480341984751,-1.81396373887019,1.8));
#9591=CARTESIAN_POINT('Origin',(-1.76776695296637,1.76776695296637,1.8));
#9592=CARTESIAN_POINT('',(-1.81396373887019,1.24480341984751,2.4));
#9593=CARTESIAN_POINT('',(-1.81396373887019,1.24480341984751,1.8));
#9594=CARTESIAN_POINT('',(-1.81396373887019,1.24480341984751,1.8));
#9595=CARTESIAN_POINT('',(-1.24480341984751,1.81396373887019,2.4));
#9596=CARTESIAN_POINT('Origin',(-1.76776695296637,1.76776695296637,2.4));
#9597=CARTESIAN_POINT('',(-1.24480341984751,1.81396373887019,1.8));
#9598=CARTESIAN_POINT('',(-1.24480341984751,1.81396373887019,1.8));
#9599=CARTESIAN_POINT('Origin',(-1.76776695296637,1.76776695296637,1.8));
#9600=CARTESIAN_POINT('Origin',(-1.76776695296637,1.76776695296637,2.4));
#9601=CARTESIAN_POINT('Origin',(0.,0.,2.4));
#9602=CARTESIAN_POINT('Origin',(1.76776695296637,1.76776695296637,1.8));
#9603=CARTESIAN_POINT('',(1.24480341984751,1.81396373887019,2.4));
#9604=CARTESIAN_POINT('',(1.24480341984751,1.81396373887019,1.8));
#9605=CARTESIAN_POINT('',(1.24480341984751,1.81396373887019,1.8));
#9606=CARTESIAN_POINT('',(1.81396373887019,1.24480341984751,2.4));
#9607=CARTESIAN_POINT('Origin',(1.76776695296637,1.76776695296637,2.4));
#9608=CARTESIAN_POINT('',(1.81396373887019,1.24480341984751,1.8));
#9609=CARTESIAN_POINT('',(1.81396373887019,1.24480341984751,1.8));
#9610=CARTESIAN_POINT('Origin',(1.76776695296637,1.76776695296637,1.8));
#9611=CARTESIAN_POINT('Origin',(1.76776695296637,1.76776695296637,2.4));
#9612=CARTESIAN_POINT('Origin',(0.,0.,2.4));
#9613=CARTESIAN_POINT('Origin',(1.76776695296637,-1.76776695296637,1.8));
#9614=CARTESIAN_POINT('',(1.81396373887019,-1.24480341984751,2.4));
#9615=CARTESIAN_POINT('',(1.81396373887019,-1.24480341984751,1.8));
#9616=CARTESIAN_POINT('',(1.81396373887019,-1.24480341984751,1.8));
#9617=CARTESIAN_POINT('',(1.24480341984751,-1.8139637388702,2.4));
#9618=CARTESIAN_POINT('Origin',(1.76776695296637,-1.76776695296637,2.4));
#9619=CARTESIAN_POINT('',(1.24480341984751,-1.8139637388702,1.8));
#9620=CARTESIAN_POINT('',(1.24480341984751,-1.8139637388702,1.8));
#9621=CARTESIAN_POINT('Origin',(1.76776695296637,-1.76776695296637,1.8));
#9622=CARTESIAN_POINT('Origin',(1.76776695296637,-1.76776695296637,2.4));
#9623=CARTESIAN_POINT('Origin',(0.,0.,2.4));
#9624=CARTESIAN_POINT('Origin',(0.,0.,1.));
#9625=CARTESIAN_POINT('',(-2.2,-2.69422295812418E-16,5.2));
#9626=CARTESIAN_POINT('Origin',(0.,0.,5.2));
#9627=CARTESIAN_POINT('',(-2.2,-2.69422295812418E-16,1.8));
#9628=CARTESIAN_POINT('',(-2.2,-2.69422295812418E-16,1.));
#9629=CARTESIAN_POINT('Origin',(0.,0.,1.8));
#9630=CARTESIAN_POINT('Origin',(0.,0.,1.8));
#9631=CARTESIAN_POINT('Origin',(0.,0.,1.8));
#9632=CARTESIAN_POINT('Origin',(0.,0.,1.8));
#9633=CARTESIAN_POINT('Origin',(0.,0.,1.8));
#9634=CARTESIAN_POINT('Origin',(0.,0.,1.8));
#9635=CARTESIAN_POINT('',(-3.,-3.67394039744206E-16,1.8));
#9636=CARTESIAN_POINT('Origin',(0.,0.,1.8));
#9637=CARTESIAN_POINT('',(-2.04276695296637,-1.76776695296637,1.8));
#9638=CARTESIAN_POINT('Origin',(-1.76776695296637,-1.76776695296637,1.8));
#9639=CARTESIAN_POINT('',(1.49276695296637,1.76776695296637,1.8));
#9640=CARTESIAN_POINT('Origin',(1.76776695296637,1.76776695296637,1.8));
#9641=CARTESIAN_POINT('',(1.49276695296637,-1.76776695296637,1.8));
#9642=CARTESIAN_POINT('Origin',(1.76776695296637,-1.76776695296637,1.8));
#9643=CARTESIAN_POINT('',(-2.04276695296637,1.76776695296637,1.8));
#9644=CARTESIAN_POINT('Origin',(-1.76776695296637,1.76776695296637,1.8));
#9645=CARTESIAN_POINT('Origin',(-1.23743686707646,-1.23743686707646,4.1));
#9646=CARTESIAN_POINT('',(-1.40243686707646,-1.23743686707646,4.1));
#9647=CARTESIAN_POINT('Origin',(-1.23743686707646,-1.23743686707646,4.1));
#9648=CARTESIAN_POINT('',(-1.40243686707646,-1.23743686707646,5.2));
#9649=CARTESIAN_POINT('',(-1.40243686707646,-1.23743686707646,4.1));
#9650=CARTESIAN_POINT('Origin',(-1.23743686707646,-1.23743686707646,5.2));
#9651=CARTESIAN_POINT('Origin',(-1.23743686707646,-1.23743686707646,4.1));
#9652=CARTESIAN_POINT('Origin',(-1.23743686707646,1.23743686707646,4.1));
#9653=CARTESIAN_POINT('',(-1.40243686707646,1.23743686707646,4.1));
#9654=CARTESIAN_POINT('Origin',(-1.23743686707646,1.23743686707646,4.1));
#9655=CARTESIAN_POINT('',(-1.40243686707646,1.23743686707646,5.2));
#9656=CARTESIAN_POINT('',(-1.40243686707646,1.23743686707646,4.1));
#9657=CARTESIAN_POINT('Origin',(-1.23743686707646,1.23743686707646,5.2));
#9658=CARTESIAN_POINT('Origin',(-1.23743686707646,1.23743686707646,4.1));
#9659=CARTESIAN_POINT('Origin',(1.23743686707646,1.23743686707646,4.1));
#9660=CARTESIAN_POINT('',(1.07243686707646,1.23743686707646,4.1));
#9661=CARTESIAN_POINT('Origin',(1.23743686707646,1.23743686707646,4.1));
#9662=CARTESIAN_POINT('',(1.07243686707646,1.23743686707646,5.2));
#9663=CARTESIAN_POINT('',(1.07243686707646,1.23743686707646,4.1));
#9664=CARTESIAN_POINT('Origin',(1.23743686707646,1.23743686707646,5.2));
#9665=CARTESIAN_POINT('Origin',(1.23743686707646,1.23743686707646,4.1));
#9666=CARTESIAN_POINT('Origin',(1.23743686707646,-1.23743686707646,4.1));
#9667=CARTESIAN_POINT('',(1.07243686707646,-1.23743686707646,4.1));
#9668=CARTESIAN_POINT('Origin',(1.23743686707646,-1.23743686707646,4.1));
#9669=CARTESIAN_POINT('',(1.07243686707646,-1.23743686707646,5.2));
#9670=CARTESIAN_POINT('',(1.07243686707646,-1.23743686707646,4.1));
#9671=CARTESIAN_POINT('Origin',(1.23743686707646,-1.23743686707646,5.2));
#9672=CARTESIAN_POINT('Origin',(1.23743686707646,-1.23743686707646,4.1));
#9673=CARTESIAN_POINT('Origin',(0.9,0.,1.4));
#9674=CARTESIAN_POINT('',(0.988888264668966,0.25,1.4));
#9675=CARTESIAN_POINT('',(1.02,-1.18386380373883E-17,1.65));
#9676=CARTESIAN_POINT('Ctrl Pts',(0.988888264668966,0.25,1.4));
#9677=CARTESIAN_POINT('Ctrl Pts',(0.988888264668966,0.25,1.43153139415882));
#9678=CARTESIAN_POINT('Ctrl Pts',(0.990553370646674,0.243672048431404,1.46507214966317));
#9679=CARTESIAN_POINT('Ctrl Pts',(0.996491737296663,0.218119830014375,1.52662620974954));
#9680=CARTESIAN_POINT('Ctrl Pts',(1.00067109353237,0.198902128206072,1.5546512623872));
#9681=CARTESIAN_POINT('Ctrl Pts',(1.00845756932386,0.154654113568716,1.59889927702456));
#9682=CARTESIAN_POINT('Ctrl Pts',(1.01258144235289,0.126627870945253,1.61811920309393));
#9683=CARTESIAN_POINT('Ctrl Pts',(1.0183917429657,0.065069600391363,1.64367304400768));
#9684=CARTESIAN_POINT('Ctrl Pts',(1.02,0.031527330883376,1.65));
#9685=CARTESIAN_POINT('Ctrl Pts',(1.02,2.77555756156289E-17,1.65));
#9686=CARTESIAN_POINT('Ctrl Pts',(1.02,6.93889390390723E-18,1.65));
#9687=CARTESIAN_POINT('Ctrl Pts',(1.02,-0.031527330883376,1.65));
#9688=CARTESIAN_POINT('Ctrl Pts',(1.0183917429657,-0.065069600391363,1.64367304400768));
#9689=CARTESIAN_POINT('Ctrl Pts',(1.01258144235289,-0.126627870945253,1.61811920309393));
#9690=CARTESIAN_POINT('Ctrl Pts',(1.00845756932386,-0.154654113568716,1.59889927702456));
#9691=CARTESIAN_POINT('Ctrl Pts',(1.00067109353237,-0.198902128206072,1.5546512623872));
#9692=CARTESIAN_POINT('Ctrl Pts',(0.996491737296663,-0.218119830014375,
1.52662620974954));
#9693=CARTESIAN_POINT('Ctrl Pts',(0.990553370646674,-0.243672048431404,
1.46507214966317));
#9694=CARTESIAN_POINT('Ctrl Pts',(0.988888264668967,-0.25,1.43153139415882));
#9695=CARTESIAN_POINT('Ctrl Pts',(0.988888264668967,-0.25,1.36846860584118));
#9696=CARTESIAN_POINT('Ctrl Pts',(0.990553370646674,-0.243672048431404,
1.33492785033683));
#9697=CARTESIAN_POINT('Ctrl Pts',(0.996491737296663,-0.218119830014375,
1.27337379025046));
#9698=CARTESIAN_POINT('Ctrl Pts',(1.00067109353237,-0.198902128206072,1.2453487376128));
#9699=CARTESIAN_POINT('Ctrl Pts',(1.00845756932386,-0.154654113568716,1.20110072297544));
#9700=CARTESIAN_POINT('Ctrl Pts',(1.01258144235289,-0.126627870945254,1.18188079690607));
#9701=CARTESIAN_POINT('Ctrl Pts',(1.0183917429657,-0.0650696003913633,1.15632695599232));
#9702=CARTESIAN_POINT('Ctrl Pts',(1.02,-0.0315273308833761,1.15));
#9703=CARTESIAN_POINT('Ctrl Pts',(1.02,0.0315273308833759,1.15));
#9704=CARTESIAN_POINT('Ctrl Pts',(1.0183917429657,0.065069600391363,1.15632695599232));
#9705=CARTESIAN_POINT('Ctrl Pts',(1.01258144235289,0.126627870945253,1.18188079690607));
#9706=CARTESIAN_POINT('Ctrl Pts',(1.00845756932386,0.154654113568716,1.20110072297544));
#9707=CARTESIAN_POINT('Ctrl Pts',(1.00067109353237,0.198902128206072,1.2453487376128));
#9708=CARTESIAN_POINT('Ctrl Pts',(0.996491737296663,0.218119830014375,1.27337379025046));
#9709=CARTESIAN_POINT('Ctrl Pts',(0.990553370646674,0.243672048431404,1.33492785033683));
#9710=CARTESIAN_POINT('Ctrl Pts',(0.988888264668967,0.25,1.36846860584118));
#9711=CARTESIAN_POINT('Ctrl Pts',(0.988888264668967,0.25,1.4));
#9712=CARTESIAN_POINT('',(3.,-3.06161699786838E-17,1.65));
#9713=CARTESIAN_POINT('',(0.9,-3.06161699786838E-17,1.65));
#9714=CARTESIAN_POINT('',(2.98956518577535,0.25,1.4));
#9715=CARTESIAN_POINT('Ctrl Pts',(2.98956518577535,0.25,1.4));
#9716=CARTESIAN_POINT('Ctrl Pts',(2.98956518577535,0.25,1.36859378633186));
#9717=CARTESIAN_POINT('Ctrl Pts',(2.99011104995181,0.24372047740942,1.33510417960069));
#9718=CARTESIAN_POINT('Ctrl Pts',(2.99208145165098,0.218202539734559,1.27351367328886));
#9719=CARTESIAN_POINT('Ctrl Pts',(2.99347740802958,0.198964922639276,1.245411532046));
#9720=CARTESIAN_POINT('Ctrl Pts',(2.99609686518216,0.154588504271054,1.20103511367778));
#9721=CARTESIAN_POINT('Ctrl Pts',(2.99749070376198,0.126486346986081,1.18179746841036));
#9722=CARTESIAN_POINT('Ctrl Pts',(2.99945625936844,0.0648957875009219,1.15627950921557));
#9723=CARTESIAN_POINT('Ctrl Pts',(3.,0.0314061622633416,1.15));
#9724=CARTESIAN_POINT('Ctrl Pts',(3.,-0.0314061622633416,1.15));
#9725=CARTESIAN_POINT('Ctrl Pts',(2.99945625936844,-0.0648957875009221,
1.15627950921557));
#9726=CARTESIAN_POINT('Ctrl Pts',(2.99749070376198,-0.126486346986081,1.18179746841036));
#9727=CARTESIAN_POINT('Ctrl Pts',(2.99609686518216,-0.154588504271054,1.20103511367778));
#9728=CARTESIAN_POINT('Ctrl Pts',(2.99347740802958,-0.198964922639276,1.245411532046));
#9729=CARTESIAN_POINT('Ctrl Pts',(2.99208145165098,-0.218202539734559,1.27351367328886));
#9730=CARTESIAN_POINT('Ctrl Pts',(2.99011104995181,-0.24372047740942,1.33510417960069));
#9731=CARTESIAN_POINT('Ctrl Pts',(2.98956518577535,-0.25,1.36859378633186));
#9732=CARTESIAN_POINT('Ctrl Pts',(2.98956518577535,-0.25,1.43140621366814));
#9733=CARTESIAN_POINT('Ctrl Pts',(2.99011104995181,-0.24372047740942,1.4648958203993));
#9734=CARTESIAN_POINT('Ctrl Pts',(2.99208145165098,-0.21820253973456,1.52648632671114));
#9735=CARTESIAN_POINT('Ctrl Pts',(2.99347740802958,-0.198964922639276,1.554588467954));
#9736=CARTESIAN_POINT('Ctrl Pts',(2.99609686518216,-0.154588504271054,1.59896488632222));
#9737=CARTESIAN_POINT('Ctrl Pts',(2.99749070376198,-0.126486346986082,1.61820253158964));
#9738=CARTESIAN_POINT('Ctrl Pts',(2.99945625936844,-0.0648957875009221,
1.64372049078443));
#9739=CARTESIAN_POINT('Ctrl Pts',(3.,-0.0314061622633417,1.65));
#9740=CARTESIAN_POINT('Ctrl Pts',(3.,-5.55111512312578E-17,1.65));
#9741=CARTESIAN_POINT('Ctrl Pts',(3.,-2.08166817117217E-17,1.65));
#9742=CARTESIAN_POINT('Ctrl Pts',(3.,0.0314061622633416,1.65));
#9743=CARTESIAN_POINT('Ctrl Pts',(2.99945625936844,0.0648957875009221,1.64372049078443));
#9744=CARTESIAN_POINT('Ctrl Pts',(2.99749070376198,0.126486346986081,1.61820253158964));
#9745=CARTESIAN_POINT('Ctrl Pts',(2.99609686518216,0.154588504271054,1.59896488632222));
#9746=CARTESIAN_POINT('Ctrl Pts',(2.99347740802958,0.198964922639276,1.554588467954));
#9747=CARTESIAN_POINT('Ctrl Pts',(2.99208145165098,0.218202539734559,1.52648632671114));
#9748=CARTESIAN_POINT('Ctrl Pts',(2.99011104995181,0.24372047740942,1.46489582039931));
#9749=CARTESIAN_POINT('Ctrl Pts',(2.98956518577535,0.25,1.43140621366814));
#9750=CARTESIAN_POINT('Ctrl Pts',(2.98956518577535,0.25,1.4));
#9751=CARTESIAN_POINT('Origin',(-1.76776695296637,-1.76776695296637,0.9));
#9752=CARTESIAN_POINT('',(-2.04276695296637,-1.76776695296637,1.));
#9753=CARTESIAN_POINT('Origin',(-1.76776695296637,-1.76776695296637,1.));
#9754=CARTESIAN_POINT('',(-2.04276695296637,-1.76776695296637,0.9));
#9755=CARTESIAN_POINT('Origin',(-1.76776695296637,1.76776695296637,0.9));
#9756=CARTESIAN_POINT('',(-2.04276695296637,1.76776695296637,1.));
#9757=CARTESIAN_POINT('Origin',(-1.76776695296637,1.76776695296637,1.));
#9758=CARTESIAN_POINT('',(-2.04276695296637,1.76776695296637,0.9));
#9759=CARTESIAN_POINT('Origin',(1.76776695296637,1.76776695296637,0.9));
#9760=CARTESIAN_POINT('',(1.49276695296637,1.76776695296637,1.));
#9761=CARTESIAN_POINT('Origin',(1.76776695296637,1.76776695296637,1.));
#9762=CARTESIAN_POINT('',(1.49276695296637,1.76776695296637,0.9));
#9763=CARTESIAN_POINT('Origin',(1.76776695296637,-1.76776695296637,0.9));
#9764=CARTESIAN_POINT('',(1.49276695296637,-1.76776695296637,1.));
#9765=CARTESIAN_POINT('Origin',(1.76776695296637,-1.76776695296637,1.));
#9766=CARTESIAN_POINT('',(1.49276695296637,-1.76776695296637,0.9));
#9767=CARTESIAN_POINT('Origin',(0.,0.,2.05));
#9768=CARTESIAN_POINT('',(-1.5,-1.83697019872103E-16,2.05));
#9769=CARTESIAN_POINT('Origin',(0.,0.,2.05));
#9770=CARTESIAN_POINT('',(-1.5,1.83697019872103E-16,5.2));
#9771=CARTESIAN_POINT('',(-1.5,-1.83697019872103E-16,2.05));
#9772=CARTESIAN_POINT('Origin',(0.,0.,5.2));
#9773=CARTESIAN_POINT('Origin',(0.,0.,2.05));
#9774=CARTESIAN_POINT('',(-1.02,-1.2491397351303E-16,2.05));
#9775=CARTESIAN_POINT('Origin',(0.,0.,2.05));
#9776=CARTESIAN_POINT('Origin',(0.,0.,1.));
#9777=CARTESIAN_POINT('',(-3.,-3.67394039744206E-16,1.));
#9778=CARTESIAN_POINT('',(-3.,-3.67394039744206E-16,1.));
#9779=CARTESIAN_POINT('Origin',(0.,0.,1.));
#9780=CARTESIAN_POINT('Origin',(0.,0.,1.));
#9781=CARTESIAN_POINT('',(-1.02,-1.2491397351303E-16,1.));
#9782=CARTESIAN_POINT('',(-1.02,-1.2491397351303E-16,1.));
#9783=CARTESIAN_POINT('Origin',(0.,0.,1.));
#9784=CARTESIAN_POINT('Origin',(0.,0.,5.2));
#9785=CARTESIAN_POINT('Origin',(0.,0.,1.));
#9786=CARTESIAN_POINT('',(0.,0.,0.));
#9787=CARTESIAN_POINT('Origin',(0.,0.,2.95));
#9788=CARTESIAN_POINT('',(-1.02,-1.2491397351303E-16,4.05));
#9789=CARTESIAN_POINT('Origin',(0.,0.,4.05));
#9790=CARTESIAN_POINT('',(-1.02,-1.2491397351303E-16,2.95));
#9791=CARTESIAN_POINT('',(-1.02,-1.2491397351303E-16,2.95));
#9792=CARTESIAN_POINT('Origin',(0.,0.,2.95));
#9793=CARTESIAN_POINT('Origin',(0.,0.,2.95));
#9794=CARTESIAN_POINT('',(-1.49,-1.82472373072956E-16,4.05));
#9795=CARTESIAN_POINT('Origin',(0.,0.,4.05));
#9796=CARTESIAN_POINT('',(-1.49,-1.82472373072956E-16,2.95));
#9797=CARTESIAN_POINT('',(-1.49,-1.82472373072956E-16,2.95));
#9798=CARTESIAN_POINT('Origin',(0.,0.,2.95));
#9799=CARTESIAN_POINT('Origin',(0.,0.,4.05));
#9800=CARTESIAN_POINT('Origin',(0.,0.,2.95));
#9801=CARTESIAN_POINT('',(0.,0.,0.));
#9802=CARTESIAN_POINT('Origin',(-1.23743686707646,-1.23743686707646,5.1));
#9803=CARTESIAN_POINT('',(-1.46243686707646,-1.23743686707646,5.2));
#9804=CARTESIAN_POINT('Origin',(-1.23743686707646,-1.23743686707646,5.2));
#9805=CARTESIAN_POINT('',(-1.46243686707646,-1.23743686707646,5.6));
#9806=CARTESIAN_POINT('',(-1.46243686707646,-1.23743686707646,5.1));
#9807=CARTESIAN_POINT('Origin',(-1.23743686707646,-1.23743686707646,5.6));
#9808=CARTESIAN_POINT('Origin',(-1.23743686707646,1.23743686707646,5.1));
#9809=CARTESIAN_POINT('',(-1.46243686707646,1.23743686707646,5.2));
#9810=CARTESIAN_POINT('Origin',(-1.23743686707646,1.23743686707646,5.2));
#9811=CARTESIAN_POINT('',(-1.46243686707646,1.23743686707646,5.6));
#9812=CARTESIAN_POINT('',(-1.46243686707646,1.23743686707646,5.1));
#9813=CARTESIAN_POINT('Origin',(-1.23743686707646,1.23743686707646,5.6));
#9814=CARTESIAN_POINT('Origin',(1.23743686707646,1.23743686707646,5.1));
#9815=CARTESIAN_POINT('',(1.01243686707646,1.23743686707646,5.2));
#9816=CARTESIAN_POINT('Origin',(1.23743686707646,1.23743686707646,5.2));
#9817=CARTESIAN_POINT('',(1.01243686707646,1.23743686707646,5.6));
#9818=CARTESIAN_POINT('',(1.01243686707646,1.23743686707646,5.1));
#9819=CARTESIAN_POINT('Origin',(1.23743686707646,1.23743686707646,5.6));
#9820=CARTESIAN_POINT('Origin',(1.23743686707646,-1.23743686707646,5.1));
#9821=CARTESIAN_POINT('',(1.01243686707646,-1.23743686707646,5.2));
#9822=CARTESIAN_POINT('Origin',(1.23743686707646,-1.23743686707646,5.2));
#9823=CARTESIAN_POINT('',(1.01243686707646,-1.23743686707646,5.6));
#9824=CARTESIAN_POINT('',(1.01243686707646,-1.23743686707646,5.1));
#9825=CARTESIAN_POINT('Origin',(1.23743686707646,-1.23743686707646,5.6));
#9826=CARTESIAN_POINT('Origin',(0.,0.,4.95));
#9827=CARTESIAN_POINT('',(-1.49,-1.82472373072956E-16,5.2));
#9828=CARTESIAN_POINT('Origin',(0.,0.,5.2));
#9829=CARTESIAN_POINT('',(-1.49,-1.82472373072956E-16,4.95));
#9830=CARTESIAN_POINT('',(-1.49,-1.82472373072956E-16,4.95));
#9831=CARTESIAN_POINT('Origin',(0.,0.,4.95));
#9832=CARTESIAN_POINT('Origin',(0.,0.,4.95));
#9833=CARTESIAN_POINT('',(-1.02,-1.2491397351303E-16,4.95));
#9834=CARTESIAN_POINT('Origin',(0.,0.,4.95));
#9835=CARTESIAN_POINT('Origin',(0.,0.,5.2));
#9836=CARTESIAN_POINT('',(-1.02,-1.2491397351303E-16,5.6));
#9837=CARTESIAN_POINT('Origin',(0.,0.,5.6));
#9838=CARTESIAN_POINT('',(-1.02,-1.2491397351303E-16,5.2));
#9839=CARTESIAN_POINT('Origin',(0.,0.,5.2));
#9840=CARTESIAN_POINT('',(-2.2,-2.69422295812418E-16,5.6));
#9841=CARTESIAN_POINT('Origin',(0.,0.,5.6));
#9842=CARTESIAN_POINT('',(-2.2,-2.69422295812418E-16,5.2));
#9843=CARTESIAN_POINT('',(-2.2,-2.69422295812418E-16,5.2));
#9844=CARTESIAN_POINT('Origin',(0.,0.,5.2));
#9845=CARTESIAN_POINT('Origin',(0.,0.,5.6));
#9846=CARTESIAN_POINT('Origin',(0.,0.,5.2));
#9847=CARTESIAN_POINT('',(0.,0.,0.));
#9848=CARTESIAN_POINT('Origin',(6.23223304703363,-1.76776695296637,2.4));
#9849=CARTESIAN_POINT('',(6.18603626112981,-1.24480341984751,2.4));
#9850=CARTESIAN_POINT('',(6.75519658015249,-1.81396373887019,2.4));
#9851=CARTESIAN_POINT('Origin',(8.,0.,2.4));
#9852=CARTESIAN_POINT('Origin',(6.23223304703363,-1.76776695296637,2.4));
#9853=CARTESIAN_POINT('Origin',(6.23223304703363,-1.76776695296637,1.8));
#9854=CARTESIAN_POINT('',(6.18603626112981,-1.24480341984751,1.8));
#9855=CARTESIAN_POINT('',(6.18603626112981,-1.24480341984751,1.8));
#9856=CARTESIAN_POINT('',(6.75519658015249,-1.81396373887019,1.8));
#9857=CARTESIAN_POINT('Origin',(6.23223304703363,-1.76776695296637,1.8));
#9858=CARTESIAN_POINT('',(6.75519658015249,-1.81396373887019,1.8));
#9859=CARTESIAN_POINT('Origin',(6.23223304703363,1.76776695296637,1.8));
#9860=CARTESIAN_POINT('',(6.18603626112981,1.24480341984751,2.4));
#9861=CARTESIAN_POINT('',(6.18603626112981,1.24480341984751,1.8));
#9862=CARTESIAN_POINT('',(6.18603626112981,1.24480341984751,1.8));
#9863=CARTESIAN_POINT('',(6.75519658015249,1.81396373887019,2.4));
#9864=CARTESIAN_POINT('Origin',(6.23223304703363,1.76776695296637,2.4));
#9865=CARTESIAN_POINT('',(6.75519658015249,1.81396373887019,1.8));
#9866=CARTESIAN_POINT('',(6.75519658015249,1.81396373887019,1.8));
#9867=CARTESIAN_POINT('Origin',(6.23223304703363,1.76776695296637,1.8));
#9868=CARTESIAN_POINT('Origin',(6.23223304703363,1.76776695296637,2.4));
#9869=CARTESIAN_POINT('Origin',(8.,0.,2.4));
#9870=CARTESIAN_POINT('Origin',(9.76776695296637,1.76776695296637,1.8));
#9871=CARTESIAN_POINT('',(9.24480341984751,1.81396373887019,2.4));
#9872=CARTESIAN_POINT('',(9.24480341984751,1.81396373887019,1.8));
#9873=CARTESIAN_POINT('',(9.24480341984751,1.81396373887019,1.8));
#9874=CARTESIAN_POINT('',(9.8139637388702,1.24480341984751,2.4));
#9875=CARTESIAN_POINT('Origin',(9.76776695296637,1.76776695296637,2.4));
#9876=CARTESIAN_POINT('',(9.81396373887019,1.24480341984751,1.8));
#9877=CARTESIAN_POINT('',(9.8139637388702,1.24480341984751,1.8));
#9878=CARTESIAN_POINT('Origin',(9.76776695296637,1.76776695296637,1.8));
#9879=CARTESIAN_POINT('Origin',(9.76776695296637,1.76776695296637,2.4));
#9880=CARTESIAN_POINT('Origin',(8.,0.,2.4));
#9881=CARTESIAN_POINT('Origin',(9.76776695296637,-1.76776695296637,1.8));
#9882=CARTESIAN_POINT('',(9.81396373887019,-1.24480341984751,2.4));
#9883=CARTESIAN_POINT('',(9.81396373887019,-1.24480341984751,1.8));
#9884=CARTESIAN_POINT('',(9.81396373887019,-1.24480341984751,1.8));
#9885=CARTESIAN_POINT('',(9.24480341984751,-1.81396373887019,2.4));
#9886=CARTESIAN_POINT('Origin',(9.76776695296637,-1.76776695296637,2.4));
#9887=CARTESIAN_POINT('',(9.24480341984751,-1.81396373887019,1.8));
#9888=CARTESIAN_POINT('',(9.24480341984751,-1.81396373887019,1.8));
#9889=CARTESIAN_POINT('Origin',(9.76776695296637,-1.76776695296637,1.8));
#9890=CARTESIAN_POINT('Origin',(9.76776695296637,-1.76776695296637,2.4));
#9891=CARTESIAN_POINT('Origin',(8.,0.,2.4));
#9892=CARTESIAN_POINT('Origin',(8.,0.,1.));
#9893=CARTESIAN_POINT('',(5.8,-2.69422295812418E-16,5.2));
#9894=CARTESIAN_POINT('Origin',(8.,0.,5.2));
#9895=CARTESIAN_POINT('',(5.8,-2.69422295812418E-16,1.8));
#9896=CARTESIAN_POINT('',(5.8,-2.69422295812418E-16,1.));
#9897=CARTESIAN_POINT('Origin',(8.,0.,1.8));
#9898=CARTESIAN_POINT('Origin',(8.,0.,1.8));
#9899=CARTESIAN_POINT('Origin',(8.,0.,1.8));
#9900=CARTESIAN_POINT('Origin',(8.,0.,1.8));
#9901=CARTESIAN_POINT('Origin',(8.,0.,1.8));
#9902=CARTESIAN_POINT('Origin',(8.,0.,1.8));
#9903=CARTESIAN_POINT('',(5.,-3.67394039744206E-16,1.8));
#9904=CARTESIAN_POINT('Origin',(8.,0.,1.8));
#9905=CARTESIAN_POINT('',(5.95723304703363,-1.76776695296637,1.8));
#9906=CARTESIAN_POINT('Origin',(6.23223304703363,-1.76776695296637,1.8));
#9907=CARTESIAN_POINT('',(9.49276695296637,1.76776695296637,1.8));
#9908=CARTESIAN_POINT('Origin',(9.76776695296637,1.76776695296637,1.8));
#9909=CARTESIAN_POINT('',(9.49276695296637,-1.76776695296637,1.8));
#9910=CARTESIAN_POINT('Origin',(9.76776695296637,-1.76776695296637,1.8));
#9911=CARTESIAN_POINT('',(5.95723304703363,1.76776695296637,1.8));
#9912=CARTESIAN_POINT('Origin',(6.23223304703363,1.76776695296637,1.8));
#9913=CARTESIAN_POINT('Origin',(6.76256313292354,-1.23743686707646,4.1));
#9914=CARTESIAN_POINT('',(6.59756313292354,-1.23743686707646,4.1));
#9915=CARTESIAN_POINT('Origin',(6.76256313292354,-1.23743686707646,4.1));
#9916=CARTESIAN_POINT('',(6.59756313292354,-1.23743686707646,5.2));
#9917=CARTESIAN_POINT('',(6.59756313292354,-1.23743686707646,4.1));
#9918=CARTESIAN_POINT('Origin',(6.76256313292354,-1.23743686707646,5.2));
#9919=CARTESIAN_POINT('Origin',(6.76256313292354,-1.23743686707646,4.1));
#9920=CARTESIAN_POINT('Origin',(6.76256313292354,1.23743686707646,4.1));
#9921=CARTESIAN_POINT('',(6.59756313292354,1.23743686707646,4.1));
#9922=CARTESIAN_POINT('Origin',(6.76256313292354,1.23743686707646,4.1));
#9923=CARTESIAN_POINT('',(6.59756313292354,1.23743686707646,5.2));
#9924=CARTESIAN_POINT('',(6.59756313292354,1.23743686707646,4.1));
#9925=CARTESIAN_POINT('Origin',(6.76256313292354,1.23743686707646,5.2));
#9926=CARTESIAN_POINT('Origin',(6.76256313292354,1.23743686707646,4.1));
#9927=CARTESIAN_POINT('Origin',(9.23743686707646,1.23743686707646,4.1));
#9928=CARTESIAN_POINT('',(9.07243686707646,1.23743686707646,4.1));
#9929=CARTESIAN_POINT('Origin',(9.23743686707646,1.23743686707646,4.1));
#9930=CARTESIAN_POINT('',(9.07243686707646,1.23743686707646,5.2));
#9931=CARTESIAN_POINT('',(9.07243686707646,1.23743686707646,4.1));
#9932=CARTESIAN_POINT('Origin',(9.23743686707646,1.23743686707646,5.2));
#9933=CARTESIAN_POINT('Origin',(9.23743686707646,1.23743686707646,4.1));
#9934=CARTESIAN_POINT('Origin',(9.23743686707646,-1.23743686707646,4.1));
#9935=CARTESIAN_POINT('',(9.07243686707646,-1.23743686707646,4.1));
#9936=CARTESIAN_POINT('Origin',(9.23743686707646,-1.23743686707646,4.1));
#9937=CARTESIAN_POINT('',(9.07243686707646,-1.23743686707646,5.2));
#9938=CARTESIAN_POINT('',(9.07243686707646,-1.23743686707646,4.1));
#9939=CARTESIAN_POINT('Origin',(9.23743686707646,-1.23743686707646,5.2));
#9940=CARTESIAN_POINT('Origin',(9.23743686707646,-1.23743686707646,4.1));
#9941=CARTESIAN_POINT('Origin',(8.9,0.,1.4));
#9942=CARTESIAN_POINT('',(8.98888826466897,0.25,1.4));
#9943=CARTESIAN_POINT('',(9.02,1.2447490626287E-17,1.65));
#9944=CARTESIAN_POINT('Ctrl Pts',(8.98888826466897,0.25,1.4));
#9945=CARTESIAN_POINT('Ctrl Pts',(8.98888826466897,0.25,1.43153139415882));
#9946=CARTESIAN_POINT('Ctrl Pts',(8.99055337064667,0.243672048431404,1.46507214966317));
#9947=CARTESIAN_POINT('Ctrl Pts',(8.99649173729666,0.218119830014375,1.52662620974954));
#9948=CARTESIAN_POINT('Ctrl Pts',(9.00067109353237,0.198902128206072,1.5546512623872));
#9949=CARTESIAN_POINT('Ctrl Pts',(9.00845756932386,0.154654113568716,1.59889927702456));
#9950=CARTESIAN_POINT('Ctrl Pts',(9.01258144235289,0.126627870945253,1.61811920309393));
#9951=CARTESIAN_POINT('Ctrl Pts',(9.0183917429657,0.0650696003913631,1.64367304400768));
#9952=CARTESIAN_POINT('Ctrl Pts',(9.02,0.031527330883376,1.65));
#9953=CARTESIAN_POINT('Ctrl Pts',(9.02,3.46944695195361E-17,1.65));
#9954=CARTESIAN_POINT('Ctrl Pts',(9.02,3.46944695195361E-17,1.65));
#9955=CARTESIAN_POINT('Ctrl Pts',(9.02,-0.0315273308833759,1.65));
#9956=CARTESIAN_POINT('Ctrl Pts',(9.0183917429657,-0.065069600391363,1.64367304400768));
#9957=CARTESIAN_POINT('Ctrl Pts',(9.01258144235289,-0.126627870945253,1.61811920309393));
#9958=CARTESIAN_POINT('Ctrl Pts',(9.00845756932386,-0.154654113568716,1.59889927702456));
#9959=CARTESIAN_POINT('Ctrl Pts',(9.00067109353237,-0.198902128206072,1.5546512623872));
#9960=CARTESIAN_POINT('Ctrl Pts',(8.99649173729666,-0.218119830014375,1.52662620974954));
#9961=CARTESIAN_POINT('Ctrl Pts',(8.99055337064667,-0.243672048431404,1.46507214966317));
#9962=CARTESIAN_POINT('Ctrl Pts',(8.98888826466897,-0.25,1.43153139415882));
#9963=CARTESIAN_POINT('Ctrl Pts',(8.98888826466897,-0.25,1.36846860584118));
#9964=CARTESIAN_POINT('Ctrl Pts',(8.99055337064667,-0.243672048431404,1.33492785033683));
#9965=CARTESIAN_POINT('Ctrl Pts',(8.99649173729666,-0.218119830014375,1.27337379025046));
#9966=CARTESIAN_POINT('Ctrl Pts',(9.00067109353237,-0.198902128206072,1.2453487376128));
#9967=CARTESIAN_POINT('Ctrl Pts',(9.00845756932386,-0.154654113568716,1.20110072297544));
#9968=CARTESIAN_POINT('Ctrl Pts',(9.01258144235289,-0.126627870945253,1.18188079690607));
#9969=CARTESIAN_POINT('Ctrl Pts',(9.0183917429657,-0.0650696003913632,1.15632695599232));
#9970=CARTESIAN_POINT('Ctrl Pts',(9.02,-0.031527330883376,1.15));
#9971=CARTESIAN_POINT('Ctrl Pts',(9.02,0.0315273308833759,1.15));
#9972=CARTESIAN_POINT('Ctrl Pts',(9.0183917429657,0.065069600391363,1.15632695599232));
#9973=CARTESIAN_POINT('Ctrl Pts',(9.01258144235289,0.126627870945253,1.18188079690607));
#9974=CARTESIAN_POINT('Ctrl Pts',(9.00845756932386,0.154654113568716,1.20110072297544));
#9975=CARTESIAN_POINT('Ctrl Pts',(9.00067109353237,0.198902128206072,1.2453487376128));
#9976=CARTESIAN_POINT('Ctrl Pts',(8.99649173729666,0.218119830014375,1.27337379025046));
#9977=CARTESIAN_POINT('Ctrl Pts',(8.99055337064667,0.243672048431404,1.33492785033683));
#9978=CARTESIAN_POINT('Ctrl Pts',(8.98888826466897,0.25,1.36846860584118));
#9979=CARTESIAN_POINT('Ctrl Pts',(8.98888826466897,0.25,1.4));
#9980=CARTESIAN_POINT('',(11.,-3.06161699786838E-17,1.65));
#9981=CARTESIAN_POINT('',(8.9,-3.06161699786838E-17,1.65));
#9982=CARTESIAN_POINT('',(10.9895651857753,0.25,1.4));
#9983=CARTESIAN_POINT('Ctrl Pts',(10.9895651857753,0.25,1.4));
#9984=CARTESIAN_POINT('Ctrl Pts',(10.9895651857753,0.25,1.36859378633186));
#9985=CARTESIAN_POINT('Ctrl Pts',(10.9901110499518,0.24372047740942,1.33510417960069));
#9986=CARTESIAN_POINT('Ctrl Pts',(10.992081451651,0.218202539734559,1.27351367328886));
#9987=CARTESIAN_POINT('Ctrl Pts',(10.9934774080296,0.198964922639276,1.245411532046));
#9988=CARTESIAN_POINT('Ctrl Pts',(10.9960968651822,0.154588504271054,1.20103511367778));
#9989=CARTESIAN_POINT('Ctrl Pts',(10.997490703762,0.126486346986081,1.18179746841036));
#9990=CARTESIAN_POINT('Ctrl Pts',(10.9994562593684,0.064895787500922,1.15627950921557));
#9991=CARTESIAN_POINT('Ctrl Pts',(11.,0.0314061622633416,1.15));
#9992=CARTESIAN_POINT('Ctrl Pts',(11.,-0.0314061622633416,1.15));
#9993=CARTESIAN_POINT('Ctrl Pts',(10.9994562593684,-0.064895787500922,1.15627950921557));
#9994=CARTESIAN_POINT('Ctrl Pts',(10.997490703762,-0.126486346986081,1.18179746841036));
#9995=CARTESIAN_POINT('Ctrl Pts',(10.9960968651822,-0.154588504271054,1.20103511367778));
#9996=CARTESIAN_POINT('Ctrl Pts',(10.9934774080296,-0.198964922639276,1.245411532046));
#9997=CARTESIAN_POINT('Ctrl Pts',(10.992081451651,-0.218202539734559,1.27351367328886));
#9998=CARTESIAN_POINT('Ctrl Pts',(10.9901110499518,-0.24372047740942,1.33510417960069));
#9999=CARTESIAN_POINT('Ctrl Pts',(10.9895651857753,-0.25,1.36859378633186));
#10000=CARTESIAN_POINT('Ctrl Pts',(10.9895651857753,-0.25,1.43140621366814));
#10001=CARTESIAN_POINT('Ctrl Pts',(10.9901110499518,-0.24372047740942,1.4648958203993));
#10002=CARTESIAN_POINT('Ctrl Pts',(10.992081451651,-0.21820253973456,1.52648632671114));
#10003=CARTESIAN_POINT('Ctrl Pts',(10.9934774080296,-0.198964922639276,
1.554588467954));
#10004=CARTESIAN_POINT('Ctrl Pts',(10.9960968651822,-0.154588504271054,
1.59896488632222));
#10005=CARTESIAN_POINT('Ctrl Pts',(10.997490703762,-0.126486346986081,1.61820253158964));
#10006=CARTESIAN_POINT('Ctrl Pts',(10.9994562593684,-0.0648957875009221,
1.64372049078443));
#10007=CARTESIAN_POINT('Ctrl Pts',(11.,-0.0314061622633417,1.65));
#10008=CARTESIAN_POINT('Ctrl Pts',(11.,-4.85722573273506E-17,1.65));
#10009=CARTESIAN_POINT('Ctrl Pts',(11.,1.38777878078145E-17,1.65));
#10010=CARTESIAN_POINT('Ctrl Pts',(11.,0.0314061622633416,1.65));
#10011=CARTESIAN_POINT('Ctrl Pts',(10.9994562593684,0.064895787500922,1.64372049078443));
#10012=CARTESIAN_POINT('Ctrl Pts',(10.997490703762,0.126486346986081,1.61820253158964));
#10013=CARTESIAN_POINT('Ctrl Pts',(10.9960968651822,0.154588504271054,1.59896488632222));
#10014=CARTESIAN_POINT('Ctrl Pts',(10.9934774080296,0.198964922639276,1.554588467954));
#10015=CARTESIAN_POINT('Ctrl Pts',(10.992081451651,0.218202539734559,1.52648632671114));
#10016=CARTESIAN_POINT('Ctrl Pts',(10.9901110499518,0.24372047740942,1.46489582039931));
#10017=CARTESIAN_POINT('Ctrl Pts',(10.9895651857753,0.25,1.43140621366814));
#10018=CARTESIAN_POINT('Ctrl Pts',(10.9895651857753,0.25,1.4));
#10019=CARTESIAN_POINT('Origin',(6.23223304703363,-1.76776695296637,0.9));
#10020=CARTESIAN_POINT('',(5.95723304703363,-1.76776695296637,1.));
#10021=CARTESIAN_POINT('Origin',(6.23223304703363,-1.76776695296637,1.));
#10022=CARTESIAN_POINT('',(5.95723304703363,-1.76776695296637,0.9));
#10023=CARTESIAN_POINT('Origin',(6.23223304703363,1.76776695296637,0.9));
#10024=CARTESIAN_POINT('',(5.95723304703363,1.76776695296637,1.));
#10025=CARTESIAN_POINT('Origin',(6.23223304703363,1.76776695296637,1.));
#10026=CARTESIAN_POINT('',(5.95723304703363,1.76776695296637,0.9));
#10027=CARTESIAN_POINT('Origin',(9.76776695296637,1.76776695296637,0.9));
#10028=CARTESIAN_POINT('',(9.49276695296637,1.76776695296637,1.));
#10029=CARTESIAN_POINT('Origin',(9.76776695296637,1.76776695296637,1.));
#10030=CARTESIAN_POINT('',(9.49276695296637,1.76776695296637,0.9));
#10031=CARTESIAN_POINT('Origin',(9.76776695296637,-1.76776695296637,0.9));
#10032=CARTESIAN_POINT('',(9.49276695296637,-1.76776695296637,1.));
#10033=CARTESIAN_POINT('Origin',(9.76776695296637,-1.76776695296637,1.));
#10034=CARTESIAN_POINT('',(9.49276695296637,-1.76776695296637,0.9));
#10035=CARTESIAN_POINT('Origin',(8.,0.,3.05));
#10036=CARTESIAN_POINT('',(6.5,-1.83697019872103E-16,3.05));
#10037=CARTESIAN_POINT('Origin',(8.,0.,3.05));
#10038=CARTESIAN_POINT('',(6.5,1.83697019872103E-16,5.2));
#10039=CARTESIAN_POINT('',(6.5,-1.83697019872103E-16,3.05));
#10040=CARTESIAN_POINT('Origin',(8.,0.,5.2));
#10041=CARTESIAN_POINT('Origin',(8.,0.,3.05));
#10042=CARTESIAN_POINT('',(6.98,-1.2491397351303E-16,3.05));
#10043=CARTESIAN_POINT('Origin',(8.,0.,3.05));
#10044=CARTESIAN_POINT('Origin',(8.,0.,1.));
#10045=CARTESIAN_POINT('',(5.,-3.67394039744206E-16,1.));
#10046=CARTESIAN_POINT('',(5.,-3.67394039744206E-16,1.));
#10047=CARTESIAN_POINT('Origin',(8.,0.,1.));
#10048=CARTESIAN_POINT('Origin',(8.,0.,1.));
#10049=CARTESIAN_POINT('',(6.98,-1.2491397351303E-16,1.));
#10050=CARTESIAN_POINT('',(6.98,-1.2491397351303E-16,1.));
#10051=CARTESIAN_POINT('Origin',(8.,0.,1.));
#10052=CARTESIAN_POINT('Origin',(8.,0.,5.2));
#10053=CARTESIAN_POINT('Origin',(8.,0.,1.));
#10054=CARTESIAN_POINT('',(0.,0.,0.));
#10055=CARTESIAN_POINT('Origin',(6.76256313292354,-1.23743686707646,5.1));
#10056=CARTESIAN_POINT('',(6.53756313292354,-1.23743686707646,5.2));
#10057=CARTESIAN_POINT('Origin',(6.76256313292354,-1.23743686707646,5.2));
#10058=CARTESIAN_POINT('',(6.53756313292354,-1.23743686707646,5.6));
#10059=CARTESIAN_POINT('',(6.53756313292354,-1.23743686707646,5.1));
#10060=CARTESIAN_POINT('Origin',(6.76256313292354,-1.23743686707646,5.6));
#10061=CARTESIAN_POINT('Origin',(6.76256313292354,1.23743686707646,5.1));
#10062=CARTESIAN_POINT('',(6.53756313292354,1.23743686707646,5.2));
#10063=CARTESIAN_POINT('Origin',(6.76256313292354,1.23743686707646,5.2));
#10064=CARTESIAN_POINT('',(6.53756313292354,1.23743686707646,5.6));
#10065=CARTESIAN_POINT('',(6.53756313292354,1.23743686707646,5.1));
#10066=CARTESIAN_POINT('Origin',(6.76256313292354,1.23743686707646,5.6));
#10067=CARTESIAN_POINT('Origin',(9.23743686707646,1.23743686707646,5.1));
#10068=CARTESIAN_POINT('',(9.01243686707646,1.23743686707646,5.2));
#10069=CARTESIAN_POINT('Origin',(9.23743686707646,1.23743686707646,5.2));
#10070=CARTESIAN_POINT('',(9.01243686707646,1.23743686707646,5.6));
#10071=CARTESIAN_POINT('',(9.01243686707646,1.23743686707646,5.1));
#10072=CARTESIAN_POINT('Origin',(9.23743686707646,1.23743686707646,5.6));
#10073=CARTESIAN_POINT('Origin',(9.23743686707646,-1.23743686707646,5.1));
#10074=CARTESIAN_POINT('',(9.01243686707646,-1.23743686707646,5.2));
#10075=CARTESIAN_POINT('Origin',(9.23743686707646,-1.23743686707646,5.2));
#10076=CARTESIAN_POINT('',(9.01243686707646,-1.23743686707646,5.6));
#10077=CARTESIAN_POINT('',(9.01243686707646,-1.23743686707646,5.1));
#10078=CARTESIAN_POINT('Origin',(9.23743686707646,-1.23743686707646,5.6));
#10079=CARTESIAN_POINT('Origin',(8.,0.,3.95));
#10080=CARTESIAN_POINT('',(6.51,-1.82472373072956E-16,5.2));
#10081=CARTESIAN_POINT('Origin',(8.,0.,5.2));
#10082=CARTESIAN_POINT('',(6.51,-1.82472373072956E-16,3.95));
#10083=CARTESIAN_POINT('',(6.51,-1.82472373072956E-16,3.95));
#10084=CARTESIAN_POINT('Origin',(8.,0.,3.95));
#10085=CARTESIAN_POINT('Origin',(8.,0.,3.95));
#10086=CARTESIAN_POINT('',(6.98,-1.2491397351303E-16,3.95));
#10087=CARTESIAN_POINT('Origin',(8.,0.,3.95));
#10088=CARTESIAN_POINT('Origin',(8.,0.,5.2));
#10089=CARTESIAN_POINT('',(6.98,-1.2491397351303E-16,5.6));
#10090=CARTESIAN_POINT('Origin',(8.,0.,5.6));
#10091=CARTESIAN_POINT('',(6.98,-1.2491397351303E-16,5.2));
#10092=CARTESIAN_POINT('Origin',(8.,0.,5.2));
#10093=CARTESIAN_POINT('',(5.8,-2.69422295812418E-16,5.6));
#10094=CARTESIAN_POINT('Origin',(8.,0.,5.6));
#10095=CARTESIAN_POINT('',(5.8,-2.69422295812418E-16,5.2));
#10096=CARTESIAN_POINT('',(5.8,-2.69422295812418E-16,5.2));
#10097=CARTESIAN_POINT('Origin',(8.,0.,5.2));
#10098=CARTESIAN_POINT('Origin',(8.,0.,5.6));
#10099=CARTESIAN_POINT('Origin',(8.,0.,5.2));
#10100=CARTESIAN_POINT('',(0.,0.,0.));
#10101=CARTESIAN_POINT('Origin',(0.115470053837925,-0.5,-0.2));
#10102=CARTESIAN_POINT('',(0.23094010767585,-0.5,0.));
#10103=CARTESIAN_POINT('',(0.115470053837925,-0.5,-0.2));
#10104=CARTESIAN_POINT('',(0.23094010767585,-0.5,0.));
#10105=CARTESIAN_POINT('',(0.115470053837925,-0.8,-0.2));
#10106=CARTESIAN_POINT('',(0.115470053837925,-0.5,-0.2));
#10107=CARTESIAN_POINT('',(0.23094010767585,-0.8,0.));
#10108=CARTESIAN_POINT('',(0.23094010767585,-0.8,0.));
#10109=CARTESIAN_POINT('',(0.23094010767585,-0.5,0.));
#10110=CARTESIAN_POINT('Origin',(-0.115470053837925,-0.5,-0.2));
#10111=CARTESIAN_POINT('',(-0.115470053837925,-0.5,-0.2));
#10112=CARTESIAN_POINT('',(0.115470053837925,-0.5,-0.2));
#10113=CARTESIAN_POINT('',(-0.115470053837925,-0.8,-0.2));
#10114=CARTESIAN_POINT('',(-0.115470053837925,-0.5,-0.2));
#10115=CARTESIAN_POINT('',(0.115470053837925,-0.8,-0.2));
#10116=CARTESIAN_POINT('Origin',(-0.23094010767585,-0.5,-2.77555756156289E-17));
#10117=CARTESIAN_POINT('',(-0.23094010767585,-0.5,-2.82820063659975E-17));
#10118=CARTESIAN_POINT('',(-0.115470053837925,-0.5,-0.2));
#10119=CARTESIAN_POINT('',(-0.23094010767585,-0.8,-2.77555756156289E-17));
#10120=CARTESIAN_POINT('',(-0.23094010767585,-0.5,-2.82820063659975E-17));
#10121=CARTESIAN_POINT('',(-0.115470053837925,-0.8,-0.2));
#10122=CARTESIAN_POINT('Origin',(-0.115470053837925,-0.5,0.2));
#10123=CARTESIAN_POINT('',(-0.115470053837925,-0.5,0.2));
#10124=CARTESIAN_POINT('',(-0.23094010767585,-0.5,-2.82820063659975E-17));
#10125=CARTESIAN_POINT('',(-0.115470053837925,-0.8,0.2));
#10126=CARTESIAN_POINT('',(-0.115470053837925,-0.5,0.2));
#10127=CARTESIAN_POINT('',(-0.23094010767585,-0.8,-2.82820063659975E-17));
#10128=CARTESIAN_POINT('Origin',(0.115470053837925,-0.5,0.2));
#10129=CARTESIAN_POINT('',(0.115470053837925,-0.5,0.2));
#10130=CARTESIAN_POINT('',(-0.115470053837925,-0.5,0.2));
#10131=CARTESIAN_POINT('',(0.115470053837925,-0.8,0.2));
#10132=CARTESIAN_POINT('',(0.115470053837925,-0.5,0.2));
#10133=CARTESIAN_POINT('',(-0.115470053837925,-0.8,0.2));
#10134=CARTESIAN_POINT('Origin',(0.23094010767585,-0.5,0.));
#10135=CARTESIAN_POINT('',(0.115470053837925,-0.5,0.2));
#10136=CARTESIAN_POINT('',(0.115470053837925,-0.8,0.2));
#10137=CARTESIAN_POINT('Origin',(0.,-0.5,0.));
#10138=CARTESIAN_POINT('Origin',(0.,-0.8,0.));
#10139=CARTESIAN_POINT('Origin',(0.,-1.4,0.));
#10140=CARTESIAN_POINT('',(-0.24505,-1.4,3.00099698131059E-17));
#10141=CARTESIAN_POINT('Origin',(0.,-1.4,0.));
#10142=CARTESIAN_POINT('Origin',(0.375,0.5,0.));
#10143=CARTESIAN_POINT('',(-0.375,0.5,-4.59242549680257E-17));
#10144=CARTESIAN_POINT('Origin',(0.,0.5,0.));
#10145=CARTESIAN_POINT('Origin',(0.,0.475,0.));
#10146=CARTESIAN_POINT('',(-0.425,0.45,-5.20474889637625E-17));
#10147=CARTESIAN_POINT('Origin',(0.,0.45,0.));
#10148=CARTESIAN_POINT('',(-0.4,0.475,-4.89858719658941E-17));
#10149=CARTESIAN_POINT('Origin',(0.,0.24,0.));
#10150=CARTESIAN_POINT('',(-0.425,0.0299999999999998,-5.20474889637625E-17));
#10151=CARTESIAN_POINT('Origin',(0.,0.0299999999999998,0.));
#10152=CARTESIAN_POINT('',(-0.425,0.24,-5.20474889637625E-17));
#10153=CARTESIAN_POINT('Origin',(0.,0.0150000000000001,0.));
#10154=CARTESIAN_POINT('',(-0.395,4.85722573273506E-17,-4.83735485663204E-17));
#10155=CARTESIAN_POINT('Origin',(0.,0.,0.));
#10156=CARTESIAN_POINT('',(-0.41,0.0150000000000001,-5.02105187650415E-17));
#10157=CARTESIAN_POINT('Origin',(0.27,0.,0.));
#10158=CARTESIAN_POINT('',(-0.27,0.,-3.30654635769785E-17));
#10159=CARTESIAN_POINT('Origin',(0.,0.,0.));
#10160=CARTESIAN_POINT('Origin',(0.,-0.02,0.));
#10161=CARTESIAN_POINT('',(-0.24505,-0.0498999999999999,3.00099698131059E-17));
#10162=CARTESIAN_POINT('Origin',(0.,-0.0498999999999999,0.));
#10163=CARTESIAN_POINT('',(-0.26,-0.02,-3.18408167778312E-17));
#10164=CARTESIAN_POINT('Origin',(0.,-0.995,0.));
#10165=CARTESIAN_POINT('',(-0.24505,-0.995,-3.00099698131059E-17));
#10166=CARTESIAN_POINT('',(0.,0.,0.));
#10167=CARTESIAN_POINT('',(0.,0.,0.));
#10168=CARTESIAN_POINT('Origin',(0.,0.,0.));
#10169=CARTESIAN_POINT('',(-0.976185,-0.246528389340863,-1.19548183562566E-16));
#10170=CARTESIAN_POINT('',(-1.19548183562566E-16,-0.246528389340863,0.976185));
#10171=CARTESIAN_POINT('Origin',(0.,-0.246528389340863,0.));
#10172=CARTESIAN_POINT('Origin',(0.,-0.246528389340863,0.));
#10173=CARTESIAN_POINT('',(-1.19548183562566E-16,0.246528389340863,0.976185));
#10174=CARTESIAN_POINT('Origin',(-1.22464679914735E-16,0.,1.));
#10175=CARTESIAN_POINT('',(-0.976185,0.246528389340863,1.19548183562566E-16));
#10176=CARTESIAN_POINT('Origin',(0.,0.246528389340863,0.));
#10177=CARTESIAN_POINT('Origin',(0.,0.246528389340863,0.));
#10178=CARTESIAN_POINT('Origin',(0.,0.,0.));
#10179=CARTESIAN_POINT('',(-0.976185,0.45,-1.19548183562566E-16));
#10180=CARTESIAN_POINT('',(-0.976185,0.,-1.19548183562566E-16));
#10181=CARTESIAN_POINT('Origin',(0.,0.45,0.));
#10182=CARTESIAN_POINT('Origin',(0.,0.,0.));
#10183=CARTESIAN_POINT('',(-0.5,-0.39,-6.12323399573677E-17));
#10184=CARTESIAN_POINT('Origin',(0.,-0.39,0.));
#10185=CARTESIAN_POINT('',(-0.5,0.39,-6.12323399573677E-17));
#10186=CARTESIAN_POINT('',(-0.5,0.,-6.12323399573677E-17));
#10187=CARTESIAN_POINT('Origin',(0.,0.39,0.));
#10188=CARTESIAN_POINT('Origin',(0.,0.42,0.));
#10189=CARTESIAN_POINT('',(-0.56,0.45,-6.85802207522518E-17));
#10190=CARTESIAN_POINT('',(-0.53,0.42,-6.49062803548097E-17));
#10191=CARTESIAN_POINT('Origin',(0.,0.45,0.));
#10192=CARTESIAN_POINT('Origin',(0.976185,0.45,0.));
#10193=CARTESIAN_POINT('Origin',(0.,0.,0.));
#10194=CARTESIAN_POINT('',(-0.976185,-0.45,-1.19548183562566E-16));
#10195=CARTESIAN_POINT('Origin',(0.,-0.45,0.));
#10196=CARTESIAN_POINT('',(-0.976185,0.,-1.19548183562566E-16));
#10197=CARTESIAN_POINT('Origin',(0.56,-0.45,0.));
#10198=CARTESIAN_POINT('',(-0.56,-0.45,-6.85802207522518E-17));
#10199=CARTESIAN_POINT('Origin',(0.,-0.45,0.));
#10200=CARTESIAN_POINT('Origin',(0.,-0.42,0.));
#10201=CARTESIAN_POINT('',(-0.53,-0.42,-6.49062803548097E-17));
#10202=CARTESIAN_POINT('',(0.,0.,0.));
#10203=CARTESIAN_POINT('Origin',(0.,0.,0.));
#10204=CARTESIAN_POINT('',(-1.023815,0.246528389340863,-1.25381176266905E-16));
#10205=CARTESIAN_POINT('',(-1.25381176266905E-16,0.246528389340863,1.023815));
#10206=CARTESIAN_POINT('Origin',(0.,0.246528389340863,0.));
#10207=CARTESIAN_POINT('Origin',(0.,0.246528389340863,0.));
#10208=CARTESIAN_POINT('',(-1.25381176266905E-16,-0.246528389340863,1.023815));
#10209=CARTESIAN_POINT('Origin',(-1.22464679914735E-16,0.,1.));
#10210=CARTESIAN_POINT('',(-1.023815,-0.246528389340863,1.25381176266905E-16));
#10211=CARTESIAN_POINT('Origin',(0.,-0.246528389340863,0.));
#10212=CARTESIAN_POINT('Origin',(0.,-0.246528389340863,0.));
#10213=CARTESIAN_POINT('Origin',(0.,0.,0.));
#10214=CARTESIAN_POINT('',(-1.023815,-0.45,-1.25381176266905E-16));
#10215=CARTESIAN_POINT('Origin',(0.,-0.45,0.));
#10216=CARTESIAN_POINT('',(-1.023815,0.,-1.25381176266905E-16));
#10217=CARTESIAN_POINT('Origin',(1.44,0.45,0.));
#10218=CARTESIAN_POINT('',(-1.44,0.45,-1.76349139077219E-16));
#10219=CARTESIAN_POINT('Origin',(0.,0.45,0.));
#10220=CARTESIAN_POINT('',(-1.023815,0.45,-1.25381176266905E-16));
#10221=CARTESIAN_POINT('Origin',(0.,0.45,0.));
#10222=CARTESIAN_POINT('Origin',(0.,0.42,0.));
#10223=CARTESIAN_POINT('',(-1.5,0.39,-1.83697019872103E-16));
#10224=CARTESIAN_POINT('Origin',(0.,0.39,0.));
#10225=CARTESIAN_POINT('',(-1.47,0.42,-1.80023079474661E-16));
#10226=CARTESIAN_POINT('Origin',(0.,0.,0.));
#10227=CARTESIAN_POINT('',(-1.5,-0.39,-1.83697019872103E-16));
#10228=CARTESIAN_POINT('Origin',(0.,-0.39,0.));
#10229=CARTESIAN_POINT('',(-1.5,0.,-1.83697019872103E-16));
#10230=CARTESIAN_POINT('Origin',(0.,-0.42,0.));
#10231=CARTESIAN_POINT('',(-1.44,-0.45,-1.76349139077219E-16));
#10232=CARTESIAN_POINT('Origin',(0.,-0.45,0.));
#10233=CARTESIAN_POINT('',(-1.47,-0.42,-1.80023079474661E-16));
#10234=CARTESIAN_POINT('Origin',(1.023815,-0.45,0.));
#10235=CARTESIAN_POINT('Origin',(0.,0.,0.));
#10236=CARTESIAN_POINT('',(-1.023815,0.,-1.25381176266905E-16));
#10237=CARTESIAN_POINT('',(0.,0.,0.));
#10238=CARTESIAN_POINT('Origin',(1.,0.,0.));
#10239=CARTESIAN_POINT('',(1.,-1.78583896120461E-33,0.23815));
#10240=CARTESIAN_POINT('',(1.,-1.78583896120461E-33,-0.23815));
#10241=CARTESIAN_POINT('Origin',(1.,0.,0.));
#10242=CARTESIAN_POINT('Origin',(0.707106781186548,0.,-0.707106781186547));
#10243=CARTESIAN_POINT('',(0.875504261126124,-1.78583896120461E-33,-0.538709301246971));
#10244=CARTESIAN_POINT('',(0.538709301246971,-1.78583896120461E-33,-0.875504261126124));
#10245=CARTESIAN_POINT('Origin',(0.707106781186548,0.,-0.707106781186547));
#10246=CARTESIAN_POINT('Origin',(6.12323399573677E-17,0.,-1.));
#10247=CARTESIAN_POINT('',(0.23815,-1.78583896120461E-33,-1.));
#10248=CARTESIAN_POINT('',(-0.23815,-1.78583896120461E-33,-1.));
#10249=CARTESIAN_POINT('Origin',(6.12323399573677E-17,0.,-1.));
#10250=CARTESIAN_POINT('Origin',(-0.707106781186547,0.,-0.707106781186548));
#10251=CARTESIAN_POINT('',(-0.538709301246971,-1.78583896120461E-33,-0.875504261126124));
#10252=CARTESIAN_POINT('',(-0.875504261126124,-1.78583896120461E-33,-0.538709301246971));
#10253=CARTESIAN_POINT('Origin',(-0.707106781186547,0.,-0.707106781186548));
#10254=CARTESIAN_POINT('Origin',(-1.,0.,-1.22464679914735E-16));
#10255=CARTESIAN_POINT('',(-1.,-1.78583896120461E-33,-0.23815));
#10256=CARTESIAN_POINT('',(-1.,-1.78583896120461E-33,0.23815));
#10257=CARTESIAN_POINT('Origin',(-1.,0.,-1.22464679914735E-16));
#10258=CARTESIAN_POINT('Origin',(-0.707106781186548,0.,0.707106781186547));
#10259=CARTESIAN_POINT('',(-0.875504261126124,-7.94881478324376E-33,0.538709301246971));
#10260=CARTESIAN_POINT('',(-0.538709301246971,4.37713686083455E-33,0.875504261126124));
#10261=CARTESIAN_POINT('Origin',(-0.707106781186548,0.,0.707106781186547));
#10262=CARTESIAN_POINT('Origin',(-1.83697019872103E-16,0.,1.));
#10263=CARTESIAN_POINT('',(-0.23815,-1.78583896120461E-33,1.));
#10264=CARTESIAN_POINT('',(0.23815,-1.78583896120461E-33,1.));
#10265=CARTESIAN_POINT('Origin',(-1.83697019872103E-16,0.,1.));
#10266=CARTESIAN_POINT('Origin',(0.707106781186547,0.,0.707106781186548));
#10267=CARTESIAN_POINT('',(0.538709301246971,-4.86732687222419E-33,0.875504261126124));
#10268=CARTESIAN_POINT('',(0.875504261126124,1.29564894981497E-33,0.538709301246971));
#10269=CARTESIAN_POINT('Origin',(0.707106781186547,0.,0.707106781186548));
#10270=CARTESIAN_POINT('',(0.,0.,0.));
#10271=CARTESIAN_POINT('Origin',(0.707106781186547,0.,0.707106781186548));
#10272=CARTESIAN_POINT('',(0.504455939115715,-0.04763,0.841298510752802));
#10273=CARTESIAN_POINT('',(0.841298510752802,-0.04763,0.504455939115715));
#10274=CARTESIAN_POINT('Ctrl Pts',(0.504455939115715,-0.04763,0.841298510752802));
#10275=CARTESIAN_POINT('Ctrl Pts',(0.508899795931835,-0.0740444353928835,
0.838633903678357));
#10276=CARTESIAN_POINT('Ctrl Pts',(0.517157748491652,-0.0999305678883309,
0.833661031856294));
#10277=CARTESIAN_POINT('Ctrl Pts',(0.537715343527944,-0.142345102874864,
0.820511285096538));
#10278=CARTESIAN_POINT('Ctrl Pts',(0.548874290046456,-0.159766064500479,
0.813159949759));
#10279=CARTESIAN_POINT('Ctrl Pts',(0.573915184558107,-0.190326085855194,
0.795684265985089));
#10280=CARTESIAN_POINT('Ctrl Pts',(0.587792702767295,-0.203463743702801,
0.78555112003688));
#10281=CARTESIAN_POINT('Ctrl Pts',(0.615966552324775,-0.224161999508995,
0.763642258217233));
#10282=CARTESIAN_POINT('Ctrl Pts',(0.631684198665438,-0.232861760990032,
0.750785745543687));
#10283=CARTESIAN_POINT('Ctrl Pts',(0.663382628119203,-0.244251601209411,
0.722929908501543));
#10284=CARTESIAN_POINT('Ctrl Pts',(0.679352081686668,-0.246942143572133,
0.707917883896095));
#10285=CARTESIAN_POINT('Ctrl Pts',(0.707917883896095,-0.246942143572133,
0.679352081686668));
#10286=CARTESIAN_POINT('Ctrl Pts',(0.722929908501543,-0.244251601209411,
0.663382628119203));
#10287=CARTESIAN_POINT('Ctrl Pts',(0.750785745543687,-0.232861760990032,
0.631684198665439));
#10288=CARTESIAN_POINT('Ctrl Pts',(0.763642258217232,-0.224161999508995,
0.615966552324775));
#10289=CARTESIAN_POINT('Ctrl Pts',(0.78555112003688,-0.203463743702801,
0.587792702767295));
#10290=CARTESIAN_POINT('Ctrl Pts',(0.795684265985088,-0.190326085855194,
0.573915184558108));
#10291=CARTESIAN_POINT('Ctrl Pts',(0.813159949759,-0.15976606450048,0.548874290046456));
#10292=CARTESIAN_POINT('Ctrl Pts',(0.820511285096538,-0.142345102874864,
0.537715343527944));
#10293=CARTESIAN_POINT('Ctrl Pts',(0.833661031856294,-0.099930567888331,
0.517157748491653));
#10294=CARTESIAN_POINT('Ctrl Pts',(0.838633903678357,-0.0740444353928835,
0.508899795931835));
#10295=CARTESIAN_POINT('Ctrl Pts',(0.841298510752801,-0.0476299999999999,
0.504455939115715));
#10296=CARTESIAN_POINT('',(0.528110872004958,-0.04763,0.871530771444223));
#10297=CARTESIAN_POINT('Origin',(0.707106781186547,-0.04763,0.707106781186548));
#10298=CARTESIAN_POINT('',(0.871530771444223,-0.04763,0.528110872004959));
#10299=CARTESIAN_POINT('Ctrl Pts',(0.871530771444223,-0.0476300000000001,
0.528110872004958));
#10300=CARTESIAN_POINT('Ctrl Pts',(0.87014664509073,-0.0609922781173483,
0.530395067942936));
#10301=CARTESIAN_POINT('Ctrl Pts',(0.868149331745851,-0.0742967091364493,
0.533674141594226));
#10302=CARTESIAN_POINT('Ctrl Pts',(0.85981294420286,-0.115492077056649,
0.54708917182331));
#10303=CARTESIAN_POINT('Ctrl Pts',(0.850993704737257,-0.141695629206859,
0.560922177770136));
#10304=CARTESIAN_POINT('Ctrl Pts',(0.830754510485543,-0.181890537957859,
0.590422647829571));
#10305=CARTESIAN_POINT('Ctrl Pts',(0.816896541396381,-0.201072148666545,
0.609616703125488));
#10306=CARTESIAN_POINT('Ctrl Pts',(0.792310597819928,-0.223955109275652,
0.641117951819998));
#10307=CARTESIAN_POINT('Ctrl Pts',(0.779109323683612,-0.232742381310829,
0.657208095763053));
#10308=CARTESIAN_POINT('Ctrl Pts',(0.750552691816206,-0.244234834628584,
0.68964083160521));
#10309=CARTESIAN_POINT('Ctrl Pts',(0.735185187071673,-0.246942143572133,
0.705971972091755));
#10310=CARTESIAN_POINT('Ctrl Pts',(0.705971972091754,-0.246942143572133,
0.735185187071673));
#10311=CARTESIAN_POINT('Ctrl Pts',(0.689640831605209,-0.244234834628584,
0.750552691816206));
#10312=CARTESIAN_POINT('Ctrl Pts',(0.657208095763052,-0.232742381310829,
0.779109323683612));
#10313=CARTESIAN_POINT('Ctrl Pts',(0.641117951819998,-0.223955109275652,
0.792310597819928));
#10314=CARTESIAN_POINT('Ctrl Pts',(0.609616703125487,-0.201072148666545,
0.816896541396382));
#10315=CARTESIAN_POINT('Ctrl Pts',(0.590422647829571,-0.181890537957858,
0.830754510485544));
#10316=CARTESIAN_POINT('Ctrl Pts',(0.560922177770135,-0.141695629206858,
0.850993704737257));
#10317=CARTESIAN_POINT('Ctrl Pts',(0.547089171823309,-0.115492077056649,
0.859812944202861));
#10318=CARTESIAN_POINT('Ctrl Pts',(0.533674141594226,-0.0742967091364491,
0.868149331745852));
#10319=CARTESIAN_POINT('Ctrl Pts',(0.530395067942936,-0.0609922781173483,
0.870146645090731));
#10320=CARTESIAN_POINT('Ctrl Pts',(0.528110872004958,-0.0476300000000001,
0.871530771444223));
#10321=CARTESIAN_POINT('Origin',(0.707106781186547,-0.04763,0.707106781186548));
#10322=CARTESIAN_POINT('Origin',(0.,-0.166705,0.));
#10323=CARTESIAN_POINT('',(0.242834539687906,-0.04763,0.989696097314));
#10324=CARTESIAN_POINT('Origin',(0.,-0.04763,0.));
#10325=CARTESIAN_POINT('',(-0.242834539687907,-0.04763,0.989696097314));
#10326=CARTESIAN_POINT('Ctrl Pts',(0.242834539687906,-0.04763,0.989696097314));
#10327=CARTESIAN_POINT('Ctrl Pts',(0.24024064412003,-0.0609922781173483,
0.990332542620729));
#10328=CARTESIAN_POINT('Ctrl Pts',(0.236509675094874,-0.0742967091364492,
0.991238884025248));
#10329=CARTESIAN_POINT('Ctrl Pts',(0.221129100087819,-0.115492077056649,
0.994830026707808));
#10330=CARTESIAN_POINT('Ctrl Pts',(0.205111543747588,-0.141695629206859,
0.998375294985966));
#10331=CARTESIAN_POINT('Ctrl Pts',(0.169940289819232,-0.181890537957859,
1.00492400591205));
#10332=CARTESIAN_POINT('Ctrl Pts',(0.1465689792446,-0.201072148666545,1.00869718865384));
#10333=CARTESIAN_POINT('Ctrl Pts',(0.106909345252087,-0.223955109275652,
1.01358704779679));
#10334=CARTESIAN_POINT('Ctrl Pts',(0.0861971848975941,-0.232742381310829,
1.0156297872271));
#10335=CARTESIAN_POINT('Ctrl Pts',(0.0430711894098822,-0.244234834628584,
1.01837060663223));
#10336=CARTESIAN_POINT('Ctrl Pts',(0.0206568624125605,-0.246942143572133,
1.019052));
#10337=CARTESIAN_POINT('Ctrl Pts',(-0.0206568624125608,-0.246942143572133,
1.019052));
#10338=CARTESIAN_POINT('Ctrl Pts',(-0.0430711894098825,-0.244234834628584,
1.01837060663223));
#10339=CARTESIAN_POINT('Ctrl Pts',(-0.0861971848975943,-0.232742381310829,
1.0156297872271));
#10340=CARTESIAN_POINT('Ctrl Pts',(-0.106909345252088,-0.223955109275652,
1.01358704779679));
#10341=CARTESIAN_POINT('Ctrl Pts',(-0.1465689792446,-0.201072148666545,
1.00869718865384));
#10342=CARTESIAN_POINT('Ctrl Pts',(-0.169940289819232,-0.181890537957859,
1.00492400591205));
#10343=CARTESIAN_POINT('Ctrl Pts',(-0.205111543747588,-0.141695629206859,
0.998375294985966));
#10344=CARTESIAN_POINT('Ctrl Pts',(-0.221129100087819,-0.115492077056649,
0.994830026707808));
#10345=CARTESIAN_POINT('Ctrl Pts',(-0.236509675094875,-0.0742967091364493,
0.991238884025248));
#10346=CARTESIAN_POINT('Ctrl Pts',(-0.24024064412003,-0.0609922781173483,
0.990332542620729));
#10347=CARTESIAN_POINT('Ctrl Pts',(-0.242834539687907,-0.04763,0.989696097314));
#10348=CARTESIAN_POINT('',(-0.528110872004959,-0.04763,0.871530771444223));
#10349=CARTESIAN_POINT('Origin',(0.,-0.04763,0.));
#10350=CARTESIAN_POINT('',(-0.871530771444223,-0.04763,0.528110872004958));
#10351=CARTESIAN_POINT('Ctrl Pts',(-0.528110872004958,-0.0476300000000001,
0.871530771444223));
#10352=CARTESIAN_POINT('Ctrl Pts',(-0.530395067942936,-0.0609922781173484,
0.87014664509073));
#10353=CARTESIAN_POINT('Ctrl Pts',(-0.533674141594226,-0.0742967091364493,
0.868149331745851));
#10354=CARTESIAN_POINT('Ctrl Pts',(-0.54708917182331,-0.115492077056649,
0.85981294420286));
#10355=CARTESIAN_POINT('Ctrl Pts',(-0.560922177770136,-0.141695629206859,
0.850993704737257));
#10356=CARTESIAN_POINT('Ctrl Pts',(-0.590422647829571,-0.181890537957859,
0.830754510485543));
#10357=CARTESIAN_POINT('Ctrl Pts',(-0.609616703125488,-0.201072148666545,
0.816896541396381));
#10358=CARTESIAN_POINT('Ctrl Pts',(-0.641117951819998,-0.223955109275652,
0.792310597819928));
#10359=CARTESIAN_POINT('Ctrl Pts',(-0.657208095763053,-0.232742381310829,
0.779109323683611));
#10360=CARTESIAN_POINT('Ctrl Pts',(-0.68964083160521,-0.244234834628584,
0.750552691816205));
#10361=CARTESIAN_POINT('Ctrl Pts',(-0.705971972091755,-0.246942143572133,
0.735185187071673));
#10362=CARTESIAN_POINT('Ctrl Pts',(-0.735185187071673,-0.246942143572133,
0.705971972091754));
#10363=CARTESIAN_POINT('Ctrl Pts',(-0.750552691816206,-0.244234834628584,
0.689640831605209));
#10364=CARTESIAN_POINT('Ctrl Pts',(-0.779109323683612,-0.232742381310829,
0.657208095763052));
#10365=CARTESIAN_POINT('Ctrl Pts',(-0.792310597819928,-0.223955109275652,
0.641117951819998));
#10366=CARTESIAN_POINT('Ctrl Pts',(-0.816896541396382,-0.201072148666545,
0.609616703125487));
#10367=CARTESIAN_POINT('Ctrl Pts',(-0.830754510485544,-0.181890537957858,
0.590422647829571));
#10368=CARTESIAN_POINT('Ctrl Pts',(-0.850993704737257,-0.141695629206858,
0.560922177770135));
#10369=CARTESIAN_POINT('Ctrl Pts',(-0.859812944202861,-0.115492077056649,
0.547089171823309));
#10370=CARTESIAN_POINT('Ctrl Pts',(-0.868149331745852,-0.0742967091364491,
0.533674141594226));
#10371=CARTESIAN_POINT('Ctrl Pts',(-0.870146645090731,-0.0609922781173483,
0.530395067942936));
#10372=CARTESIAN_POINT('Ctrl Pts',(-0.871530771444223,-0.04763,0.528110872004958));
#10373=CARTESIAN_POINT('',(-0.989696097314,-0.04763,0.242834539687906));
#10374=CARTESIAN_POINT('Origin',(0.,-0.04763,0.));
#10375=CARTESIAN_POINT('',(-1.019052,-0.246942143572133,1.248489836334E-16));
#10376=CARTESIAN_POINT('Ctrl Pts',(-0.989696097314,-0.04763,0.242834539687906));
#10377=CARTESIAN_POINT('Ctrl Pts',(-0.990332542620729,-0.0609922781173483,
0.24024064412003));
#10378=CARTESIAN_POINT('Ctrl Pts',(-0.991238884025248,-0.0742967091364492,
0.236509675094874));
#10379=CARTESIAN_POINT('Ctrl Pts',(-0.994830026707808,-0.115492077056649,
0.221129100087819));
#10380=CARTESIAN_POINT('Ctrl Pts',(-0.998375294985966,-0.141695629206859,
0.205111543747588));
#10381=CARTESIAN_POINT('Ctrl Pts',(-1.00492400591205,-0.181890537957859,
0.169940289819232));
#10382=CARTESIAN_POINT('Ctrl Pts',(-1.00869718865384,-0.201072148666545,
0.1465689792446));
#10383=CARTESIAN_POINT('Ctrl Pts',(-1.01358704779679,-0.223955109275652,
0.106909345252088));
#10384=CARTESIAN_POINT('Ctrl Pts',(-1.0156297872271,-0.232742381310829,
0.0861971848975944));
#10385=CARTESIAN_POINT('Ctrl Pts',(-1.01837060663223,-0.244234834628584,
0.0430711894098825));
#10386=CARTESIAN_POINT('Ctrl Pts',(-1.019052,-0.246942143572133,0.0206568624125608));
#10387=CARTESIAN_POINT('Ctrl Pts',(-1.019052,-0.246942143572133,1.2490009027033E-16));
#10388=CARTESIAN_POINT('',(-1.019052,-0.28578,1.24797876996471E-16));
#10389=CARTESIAN_POINT('',(-1.019052,-0.166705,1.24797876996471E-16));
#10390=CARTESIAN_POINT('Origin',(0.,-0.28578,0.));
#10391=CARTESIAN_POINT('',(-0.989696097314,-0.04763,-0.242834539687906));
#10392=CARTESIAN_POINT('Ctrl Pts',(-1.019052,-0.246942143572133,1.2490009027033E-16));
#10393=CARTESIAN_POINT('Ctrl Pts',(-1.019052,-0.246942143572133,-0.0206568624125605));
#10394=CARTESIAN_POINT('Ctrl Pts',(-1.01837060663223,-0.244234834628584,
-0.0430711894098822));
#10395=CARTESIAN_POINT('Ctrl Pts',(-1.0156297872271,-0.232742381310829,
-0.0861971848975941));
#10396=CARTESIAN_POINT('Ctrl Pts',(-1.01358704779679,-0.223955109275652,
-0.106909345252087));
#10397=CARTESIAN_POINT('Ctrl Pts',(-1.00869718865384,-0.201072148666546,
-0.1465689792446));
#10398=CARTESIAN_POINT('Ctrl Pts',(-1.00492400591205,-0.181890537957859,
-0.169940289819232));
#10399=CARTESIAN_POINT('Ctrl Pts',(-0.998375294985966,-0.141695629206859,
-0.205111543747588));
#10400=CARTESIAN_POINT('Ctrl Pts',(-0.994830026707808,-0.11549207705665,
-0.221129100087819));
#10401=CARTESIAN_POINT('Ctrl Pts',(-0.991238884025248,-0.0742967091364495,
-0.236509675094874));
#10402=CARTESIAN_POINT('Ctrl Pts',(-0.990332542620729,-0.0609922781173484,
-0.24024064412003));
#10403=CARTESIAN_POINT('Ctrl Pts',(-0.989696097314,-0.0476300000000001,
-0.242834539687907));
#10404=CARTESIAN_POINT('',(-0.871530771444223,-0.04763,-0.528110872004958));
#10405=CARTESIAN_POINT('Origin',(0.,-0.04763,0.));
#10406=CARTESIAN_POINT('',(-0.528110872004958,-0.04763,-0.871530771444223));
#10407=CARTESIAN_POINT('Ctrl Pts',(-0.871530771444223,-0.0476300000000001,
-0.528110872004958));
#10408=CARTESIAN_POINT('Ctrl Pts',(-0.87014664509073,-0.0609922781173484,
-0.530395067942936));
#10409=CARTESIAN_POINT('Ctrl Pts',(-0.868149331745851,-0.0742967091364494,
-0.533674141594226));
#10410=CARTESIAN_POINT('Ctrl Pts',(-0.85981294420286,-0.115492077056649,
-0.54708917182331));
#10411=CARTESIAN_POINT('Ctrl Pts',(-0.850993704737257,-0.141695629206859,
-0.560922177770136));
#10412=CARTESIAN_POINT('Ctrl Pts',(-0.830754510485543,-0.181890537957859,
-0.590422647829571));
#10413=CARTESIAN_POINT('Ctrl Pts',(-0.816896541396381,-0.201072148666546,
-0.609616703125488));
#10414=CARTESIAN_POINT('Ctrl Pts',(-0.792310597819928,-0.223955109275652,
-0.641117951819999));
#10415=CARTESIAN_POINT('Ctrl Pts',(-0.779109323683611,-0.232742381310829,
-0.657208095763053));
#10416=CARTESIAN_POINT('Ctrl Pts',(-0.750552691816205,-0.244234834628584,
-0.68964083160521));
#10417=CARTESIAN_POINT('Ctrl Pts',(-0.735185187071673,-0.246942143572133,
-0.705971972091755));
#10418=CARTESIAN_POINT('Ctrl Pts',(-0.705971972091754,-0.246942143572133,
-0.735185187071673));
#10419=CARTESIAN_POINT('Ctrl Pts',(-0.68964083160521,-0.244234834628584,
-0.750552691816206));
#10420=CARTESIAN_POINT('Ctrl Pts',(-0.657208095763052,-0.232742381310829,
-0.779109323683612));
#10421=CARTESIAN_POINT('Ctrl Pts',(-0.641117951819998,-0.223955109275652,
-0.792310597819928));
#10422=CARTESIAN_POINT('Ctrl Pts',(-0.609616703125488,-0.201072148666545,
-0.816896541396381));
#10423=CARTESIAN_POINT('Ctrl Pts',(-0.590422647829571,-0.181890537957859,
-0.830754510485543));
#10424=CARTESIAN_POINT('Ctrl Pts',(-0.560922177770136,-0.141695629206859,
-0.850993704737257));
#10425=CARTESIAN_POINT('Ctrl Pts',(-0.54708917182331,-0.115492077056649,
-0.85981294420286));
#10426=CARTESIAN_POINT('Ctrl Pts',(-0.533674141594226,-0.0742967091364494,
-0.868149331745852));
#10427=CARTESIAN_POINT('Ctrl Pts',(-0.530395067942936,-0.0609922781173484,
-0.870146645090731));
#10428=CARTESIAN_POINT('Ctrl Pts',(-0.528110872004958,-0.0476300000000001,
-0.871530771444223));
#10429=CARTESIAN_POINT('',(-0.242834539687906,-0.04763,-0.989696097314));
#10430=CARTESIAN_POINT('Origin',(0.,-0.04763,0.));
#10431=CARTESIAN_POINT('',(0.242834539687906,-0.04763,-0.989696097314));
#10432=CARTESIAN_POINT('Ctrl Pts',(-0.242834539687907,-0.04763,-0.989696097314));
#10433=CARTESIAN_POINT('Ctrl Pts',(-0.24024064412003,-0.0609922781173483,
-0.990332542620729));
#10434=CARTESIAN_POINT('Ctrl Pts',(-0.236509675094874,-0.0742967091364493,
-0.991238884025248));
#10435=CARTESIAN_POINT('Ctrl Pts',(-0.221129100087819,-0.115492077056649,
-0.994830026707808));
#10436=CARTESIAN_POINT('Ctrl Pts',(-0.205111543747588,-0.141695629206859,
-0.998375294985966));
#10437=CARTESIAN_POINT('Ctrl Pts',(-0.169940289819232,-0.181890537957859,
-1.00492400591205));
#10438=CARTESIAN_POINT('Ctrl Pts',(-0.1465689792446,-0.201072148666545,
-1.00869718865384));
#10439=CARTESIAN_POINT('Ctrl Pts',(-0.106909345252087,-0.223955109275652,
-1.01358704779679));
#10440=CARTESIAN_POINT('Ctrl Pts',(-0.0861971848975942,-0.232742381310829,
-1.0156297872271));
#10441=CARTESIAN_POINT('Ctrl Pts',(-0.0430711894098823,-0.244234834628584,
-1.01837060663223));
#10442=CARTESIAN_POINT('Ctrl Pts',(-0.0206568624125606,-0.246942143572133,
-1.019052));
#10443=CARTESIAN_POINT('Ctrl Pts',(0.0206568624125607,-0.246942143572133,
-1.019052));
#10444=CARTESIAN_POINT('Ctrl Pts',(0.0430711894098824,-0.244234834628584,
-1.01837060663223));
#10445=CARTESIAN_POINT('Ctrl Pts',(0.0861971848975943,-0.232742381310829,
-1.0156297872271));
#10446=CARTESIAN_POINT('Ctrl Pts',(0.106909345252088,-0.223955109275652,
-1.01358704779679));
#10447=CARTESIAN_POINT('Ctrl Pts',(0.1465689792446,-0.201072148666545,-1.00869718865384));
#10448=CARTESIAN_POINT('Ctrl Pts',(0.169940289819232,-0.181890537957859,
-1.00492400591205));
#10449=CARTESIAN_POINT('Ctrl Pts',(0.205111543747588,-0.141695629206859,
-0.998375294985966));
#10450=CARTESIAN_POINT('Ctrl Pts',(0.221129100087819,-0.115492077056649,
-0.994830026707808));
#10451=CARTESIAN_POINT('Ctrl Pts',(0.236509675094874,-0.0742967091364493,
-0.991238884025248));
#10452=CARTESIAN_POINT('Ctrl Pts',(0.24024064412003,-0.0609922781173484,
-0.990332542620729));
#10453=CARTESIAN_POINT('Ctrl Pts',(0.242834539687907,-0.04763,-0.989696097314));
#10454=CARTESIAN_POINT('',(0.528110872004958,-0.04763,-0.871530771444223));
#10455=CARTESIAN_POINT('Origin',(0.,-0.04763,0.));
#10456=CARTESIAN_POINT('',(0.871530771444223,-0.04763,-0.528110872004958));
#10457=CARTESIAN_POINT('Ctrl Pts',(0.528110872004958,-0.0476300000000001,
-0.871530771444223));
#10458=CARTESIAN_POINT('Ctrl Pts',(0.530395067942936,-0.0609922781173484,
-0.870146645090731));
#10459=CARTESIAN_POINT('Ctrl Pts',(0.533674141594226,-0.0742967091364493,
-0.868149331745851));
#10460=CARTESIAN_POINT('Ctrl Pts',(0.54708917182331,-0.115492077056649,
-0.85981294420286));
#10461=CARTESIAN_POINT('Ctrl Pts',(0.560922177770136,-0.141695629206859,
-0.850993704737257));
#10462=CARTESIAN_POINT('Ctrl Pts',(0.590422647829571,-0.181890537957859,
-0.830754510485543));
#10463=CARTESIAN_POINT('Ctrl Pts',(0.609616703125488,-0.201072148666545,
-0.816896541396381));
#10464=CARTESIAN_POINT('Ctrl Pts',(0.641117951819998,-0.223955109275652,
-0.792310597819928));
#10465=CARTESIAN_POINT('Ctrl Pts',(0.657208095763053,-0.232742381310829,
-0.779109323683612));
#10466=CARTESIAN_POINT('Ctrl Pts',(0.68964083160521,-0.244234834628584,
-0.750552691816206));
#10467=CARTESIAN_POINT('Ctrl Pts',(0.705971972091755,-0.246942143572133,
-0.735185187071673));
#10468=CARTESIAN_POINT('Ctrl Pts',(0.735185187071673,-0.246942143572133,
-0.705971972091754));
#10469=CARTESIAN_POINT('Ctrl Pts',(0.750552691816206,-0.244234834628584,
-0.68964083160521));
#10470=CARTESIAN_POINT('Ctrl Pts',(0.779109323683612,-0.232742381310829,
-0.657208095763053));
#10471=CARTESIAN_POINT('Ctrl Pts',(0.792310597819928,-0.223955109275652,
-0.641117951819998));
#10472=CARTESIAN_POINT('Ctrl Pts',(0.816896541396381,-0.201072148666545,
-0.609616703125488));
#10473=CARTESIAN_POINT('Ctrl Pts',(0.830754510485543,-0.181890537957859,
-0.590422647829571));
#10474=CARTESIAN_POINT('Ctrl Pts',(0.850993704737257,-0.141695629206859,
-0.560922177770136));
#10475=CARTESIAN_POINT('Ctrl Pts',(0.85981294420286,-0.115492077056649,
-0.54708917182331));
#10476=CARTESIAN_POINT('Ctrl Pts',(0.868149331745851,-0.0742967091364493,
-0.533674141594226));
#10477=CARTESIAN_POINT('Ctrl Pts',(0.870146645090731,-0.0609922781173484,
-0.530395067942936));
#10478=CARTESIAN_POINT('Ctrl Pts',(0.871530771444223,-0.0476300000000001,
-0.528110872004958));
#10479=CARTESIAN_POINT('',(0.989696097314,-0.04763,-0.242834539687906));
#10480=CARTESIAN_POINT('Origin',(0.,-0.04763,0.));
#10481=CARTESIAN_POINT('',(0.989696097314,-0.04763,0.242834539687906));
#10482=CARTESIAN_POINT('Ctrl Pts',(0.989696097314,-0.04763,-0.242834539687907));
#10483=CARTESIAN_POINT('Ctrl Pts',(0.990332542620729,-0.0609922781173483,
-0.24024064412003));
#10484=CARTESIAN_POINT('Ctrl Pts',(0.991238884025248,-0.0742967091364493,
-0.236509675094874));
#10485=CARTESIAN_POINT('Ctrl Pts',(0.994830026707808,-0.115492077056649,
-0.221129100087819));
#10486=CARTESIAN_POINT('Ctrl Pts',(0.998375294985966,-0.141695629206859,
-0.205111543747588));
#10487=CARTESIAN_POINT('Ctrl Pts',(1.00492400591205,-0.181890537957859,
-0.169940289819232));
#10488=CARTESIAN_POINT('Ctrl Pts',(1.00869718865384,-0.201072148666545,
-0.1465689792446));
#10489=CARTESIAN_POINT('Ctrl Pts',(1.01358704779679,-0.223955109275652,
-0.106909345252087));
#10490=CARTESIAN_POINT('Ctrl Pts',(1.0156297872271,-0.232742381310829,-0.0861971848975942));
#10491=CARTESIAN_POINT('Ctrl Pts',(1.01837060663223,-0.244234834628584,
-0.0430711894098823));
#10492=CARTESIAN_POINT('Ctrl Pts',(1.019052,-0.246942143572133,-0.0206568624125607));
#10493=CARTESIAN_POINT('Ctrl Pts',(1.019052,-0.246942143572133,0.0206568624125607));
#10494=CARTESIAN_POINT('Ctrl Pts',(1.01837060663223,-0.244234834628584,
0.0430711894098823));
#10495=CARTESIAN_POINT('Ctrl Pts',(1.0156297872271,-0.232742381310829,0.0861971848975942));
#10496=CARTESIAN_POINT('Ctrl Pts',(1.01358704779679,-0.223955109275652,
0.106909345252087));
#10497=CARTESIAN_POINT('Ctrl Pts',(1.00869718865384,-0.201072148666545,
0.1465689792446));
#10498=CARTESIAN_POINT('Ctrl Pts',(1.00492400591205,-0.181890537957859,
0.169940289819232));
#10499=CARTESIAN_POINT('Ctrl Pts',(0.998375294985966,-0.141695629206859,
0.205111543747588));
#10500=CARTESIAN_POINT('Ctrl Pts',(0.994830026707808,-0.115492077056649,
0.221129100087819));
#10501=CARTESIAN_POINT('Ctrl Pts',(0.991238884025248,-0.0742967091364492,
0.236509675094874));
#10502=CARTESIAN_POINT('Ctrl Pts',(0.990332542620729,-0.0609922781173483,
0.24024064412003));
#10503=CARTESIAN_POINT('Ctrl Pts',(0.989696097314,-0.04763,0.242834539687907));
#10504=CARTESIAN_POINT('Origin',(0.,-0.04763,0.));
#10505=CARTESIAN_POINT('Origin',(0.,-0.04763,0.));
#10506=CARTESIAN_POINT('',(0.238183666596899,-0.04763,0.951592097314));
#10507=CARTESIAN_POINT('Origin',(0.,-0.04763,0.));
#10508=CARTESIAN_POINT('Origin',(-1.94289029309402E-16,-0.04763,1.));
#10509=CARTESIAN_POINT('Origin',(-1.94289029309402E-16,0.,1.));
#10510=CARTESIAN_POINT('',(-0.2381836665969,-0.04763,0.951592097314));
#10511=CARTESIAN_POINT('Ctrl Pts',(-0.238183666596899,-0.0476299999999999,
0.951592097314));
#10512=CARTESIAN_POINT('Ctrl Pts',(-0.233157223576062,-0.0740444353928835,
0.952850216871763));
#10513=CARTESIAN_POINT('Ctrl Pts',(-0.223801617934946,-0.0999305678883309,
0.955173119738174));
#10514=CARTESIAN_POINT('Ctrl Pts',(-0.199966927975188,-0.142345102874864,
0.960411259488514));
#10515=CARTESIAN_POINT('Ctrl Pts',(-0.1868781821531,-0.159766064500479,
0.963103647174702));
#10516=CARTESIAN_POINT('Ctrl Pts',(-0.15681442133453,-0.190326085855194,
0.968453058988463));
#10517=CARTESIAN_POINT('Ctrl Pts',(-0.139836317888043,-0.203463743702801,
0.971100730005489));
#10518=CARTESIAN_POINT('Ctrl Pts',(-0.104422493053067,-0.224161999508995,
0.975530745318961));
#10519=CARTESIAN_POINT('Ctrl Pts',(-0.0842175114474176,-0.232861760990032,
0.977553872336861));
#10520=CARTESIAN_POINT('Ctrl Pts',(-0.0421062857595701,-0.244251601209411,
0.980270995488453));
#10521=CARTESIAN_POINT('Ctrl Pts',(-0.0201990724523197,-0.246942143572133,
0.980948));
#10522=CARTESIAN_POINT('Ctrl Pts',(0.020199072452319,-0.246942143572133,
0.980948));
#10523=CARTESIAN_POINT('Ctrl Pts',(0.0421062857595694,-0.244251601209411,
0.980270995488454));
#10524=CARTESIAN_POINT('Ctrl Pts',(0.0842175114474169,-0.232861760990032,
0.977553872336861));
#10525=CARTESIAN_POINT('Ctrl Pts',(0.104422493053067,-0.224161999508995,
0.975530745318961));
#10526=CARTESIAN_POINT('Ctrl Pts',(0.139836317888042,-0.203463743702801,
0.971100730005489));
#10527=CARTESIAN_POINT('Ctrl Pts',(0.15681442133453,-0.190326085855194,
0.968453058988463));
#10528=CARTESIAN_POINT('Ctrl Pts',(0.1868781821531,-0.15976606450048,0.963103647174702));
#10529=CARTESIAN_POINT('Ctrl Pts',(0.199966927975188,-0.142345102874864,
0.960411259488514));
#10530=CARTESIAN_POINT('Ctrl Pts',(0.223801617934945,-0.0999305678883309,
0.955173119738174));
#10531=CARTESIAN_POINT('Ctrl Pts',(0.233157223576061,-0.0740444353928835,
0.952850216871763));
#10532=CARTESIAN_POINT('Ctrl Pts',(0.238183666596899,-0.0476299999999999,
0.951592097314));
#10533=CARTESIAN_POINT('Origin',(-1.94289029309402E-16,-0.04763,1.));
#10534=CARTESIAN_POINT('Origin',(0.,-0.04763,0.));
#10535=CARTESIAN_POINT('',(-0.504455939115715,-0.04763,0.841298510752802));
#10536=CARTESIAN_POINT('Origin',(0.,-0.04763,0.));
#10537=CARTESIAN_POINT('Origin',(-0.707106781186548,-0.04763,0.707106781186547));
#10538=CARTESIAN_POINT('Origin',(-0.707106781186548,0.,0.707106781186547));
#10539=CARTESIAN_POINT('',(-0.841298510752802,-0.04763,0.504455939115715));
#10540=CARTESIAN_POINT('Ctrl Pts',(-0.841298510752802,-0.04763,0.504455939115715));
#10541=CARTESIAN_POINT('Ctrl Pts',(-0.838633903678357,-0.0740444353928835,
0.508899795931835));
#10542=CARTESIAN_POINT('Ctrl Pts',(-0.833661031856294,-0.0999305678883309,
0.517157748491652));
#10543=CARTESIAN_POINT('Ctrl Pts',(-0.820511285096538,-0.142345102874864,
0.537715343527944));
#10544=CARTESIAN_POINT('Ctrl Pts',(-0.813159949759,-0.159766064500479,0.548874290046456));
#10545=CARTESIAN_POINT('Ctrl Pts',(-0.795684265985089,-0.190326085855194,
0.573915184558107));
#10546=CARTESIAN_POINT('Ctrl Pts',(-0.78555112003688,-0.203463743702801,
0.587792702767295));
#10547=CARTESIAN_POINT('Ctrl Pts',(-0.763642258217233,-0.224161999508995,
0.615966552324775));
#10548=CARTESIAN_POINT('Ctrl Pts',(-0.750785745543687,-0.232861760990032,
0.631684198665438));
#10549=CARTESIAN_POINT('Ctrl Pts',(-0.722929908501543,-0.244251601209411,
0.663382628119203));
#10550=CARTESIAN_POINT('Ctrl Pts',(-0.707917883896095,-0.246942143572133,
0.679352081686668));
#10551=CARTESIAN_POINT('Ctrl Pts',(-0.679352081686668,-0.246942143572133,
0.707917883896095));
#10552=CARTESIAN_POINT('Ctrl Pts',(-0.663382628119203,-0.244251601209411,
0.722929908501544));
#10553=CARTESIAN_POINT('Ctrl Pts',(-0.631684198665438,-0.232861760990031,
0.750785745543687));
#10554=CARTESIAN_POINT('Ctrl Pts',(-0.615966552324775,-0.224161999508995,
0.763642258217233));
#10555=CARTESIAN_POINT('Ctrl Pts',(-0.587792702767295,-0.203463743702801,
0.78555112003688));
#10556=CARTESIAN_POINT('Ctrl Pts',(-0.573915184558107,-0.190326085855194,
0.795684265985088));
#10557=CARTESIAN_POINT('Ctrl Pts',(-0.548874290046456,-0.159766064500479,
0.813159949759));
#10558=CARTESIAN_POINT('Ctrl Pts',(-0.537715343527944,-0.142345102874864,
0.820511285096538));
#10559=CARTESIAN_POINT('Ctrl Pts',(-0.517157748491652,-0.0999305678883309,
0.833661031856294));
#10560=CARTESIAN_POINT('Ctrl Pts',(-0.508899795931835,-0.0740444353928835,
0.838633903678357));
#10561=CARTESIAN_POINT('Ctrl Pts',(-0.504455939115716,-0.04763,0.841298510752801));
#10562=CARTESIAN_POINT('Origin',(-0.707106781186548,-0.04763,0.707106781186547));
#10563=CARTESIAN_POINT('Origin',(0.,-0.04763,0.));
#10564=CARTESIAN_POINT('',(-0.951592097314,-0.04763,0.238183666596899));
#10565=CARTESIAN_POINT('Origin',(0.,-0.04763,0.));
#10566=CARTESIAN_POINT('Origin',(-1.,-0.04763,-1.11022302462516E-16));
#10567=CARTESIAN_POINT('Origin',(-1.,0.,-1.11022302462516E-16));
#10568=CARTESIAN_POINT('',(-0.951592097314,-0.04763,-0.2381836665969));
#10569=CARTESIAN_POINT('',(-0.980948,-0.246942143572133,1.08514323328844E-18));
#10570=CARTESIAN_POINT('Ctrl Pts',(-0.951592097314,-0.04763,-0.238183666596899));
#10571=CARTESIAN_POINT('Ctrl Pts',(-0.952850216871763,-0.0740444353928835,
-0.233157223576062));
#10572=CARTESIAN_POINT('Ctrl Pts',(-0.955173119738174,-0.0999305678883309,
-0.223801617934946));
#10573=CARTESIAN_POINT('Ctrl Pts',(-0.960411259488514,-0.142345102874864,
-0.199966927975188));
#10574=CARTESIAN_POINT('Ctrl Pts',(-0.963103647174702,-0.159766064500479,
-0.1868781821531));
#10575=CARTESIAN_POINT('Ctrl Pts',(-0.968453058988463,-0.190326085855194,
-0.15681442133453));
#10576=CARTESIAN_POINT('Ctrl Pts',(-0.971100730005489,-0.203463743702801,
-0.139836317888043));
#10577=CARTESIAN_POINT('Ctrl Pts',(-0.975530745318961,-0.224161999508995,
-0.104422493053067));
#10578=CARTESIAN_POINT('Ctrl Pts',(-0.977553872336861,-0.232861760990032,
-0.0842175114474175));
#10579=CARTESIAN_POINT('Ctrl Pts',(-0.980270995488453,-0.244251601209411,
-0.0421062857595699));
#10580=CARTESIAN_POINT('Ctrl Pts',(-0.980948,-0.246942143572133,-0.0201990724523195));
#10581=CARTESIAN_POINT('Ctrl Pts',(-0.980948,-0.246942143572133,-1.17961196366423E-16));
#10582=CARTESIAN_POINT('Origin',(-1.,-0.04763,-1.11022302462516E-16));
#10583=CARTESIAN_POINT('Ctrl Pts',(-0.980948,-0.246942143572133,-1.17961196366423E-16));
#10584=CARTESIAN_POINT('Ctrl Pts',(-0.980948,-0.246942143572133,0.0201990724523192));
#10585=CARTESIAN_POINT('Ctrl Pts',(-0.980270995488453,-0.244251601209411,
0.0421062857595695));
#10586=CARTESIAN_POINT('Ctrl Pts',(-0.977553872336861,-0.232861760990032,
0.0842175114474169));
#10587=CARTESIAN_POINT('Ctrl Pts',(-0.975530745318961,-0.224161999508995,
0.104422493053066));
#10588=CARTESIAN_POINT('Ctrl Pts',(-0.971100730005489,-0.203463743702801,
0.139836317888042));
#10589=CARTESIAN_POINT('Ctrl Pts',(-0.968453058988463,-0.190326085855194,
0.15681442133453));
#10590=CARTESIAN_POINT('Ctrl Pts',(-0.963103647174702,-0.15976606450048,
0.1868781821531));
#10591=CARTESIAN_POINT('Ctrl Pts',(-0.960411259488514,-0.142345102874864,
0.199966927975188));
#10592=CARTESIAN_POINT('Ctrl Pts',(-0.955173119738174,-0.099930567888331,
0.223801617934945));
#10593=CARTESIAN_POINT('Ctrl Pts',(-0.952850216871763,-0.0740444353928835,
0.233157223576061));
#10594=CARTESIAN_POINT('Ctrl Pts',(-0.951592097314,-0.04763,0.238183666596899));
#10595=CARTESIAN_POINT('Origin',(0.,-0.04763,0.));
#10596=CARTESIAN_POINT('',(-0.841298510752802,-0.04763,-0.504455939115715));
#10597=CARTESIAN_POINT('Origin',(0.,-0.04763,0.));
#10598=CARTESIAN_POINT('Origin',(-0.707106781186547,-0.04763,-0.707106781186548));
#10599=CARTESIAN_POINT('Origin',(-0.707106781186547,0.,-0.707106781186548));
#10600=CARTESIAN_POINT('',(-0.504455939115715,-0.04763,-0.841298510752802));
#10601=CARTESIAN_POINT('Ctrl Pts',(-0.504455939115715,-0.04763,-0.841298510752802));
#10602=CARTESIAN_POINT('Ctrl Pts',(-0.508899795931835,-0.0740444353928835,
-0.838633903678357));
#10603=CARTESIAN_POINT('Ctrl Pts',(-0.517157748491652,-0.0999305678883309,
-0.833661031856294));
#10604=CARTESIAN_POINT('Ctrl Pts',(-0.537715343527944,-0.142345102874864,
-0.820511285096538));
#10605=CARTESIAN_POINT('Ctrl Pts',(-0.548874290046456,-0.159766064500479,
-0.813159949759));
#10606=CARTESIAN_POINT('Ctrl Pts',(-0.573915184558107,-0.190326085855194,
-0.795684265985089));
#10607=CARTESIAN_POINT('Ctrl Pts',(-0.587792702767295,-0.203463743702801,
-0.78555112003688));
#10608=CARTESIAN_POINT('Ctrl Pts',(-0.615966552324775,-0.224161999508995,
-0.763642258217233));
#10609=CARTESIAN_POINT('Ctrl Pts',(-0.631684198665438,-0.232861760990032,
-0.750785745543687));
#10610=CARTESIAN_POINT('Ctrl Pts',(-0.663382628119203,-0.244251601209411,
-0.722929908501543));
#10611=CARTESIAN_POINT('Ctrl Pts',(-0.679352081686668,-0.246942143572133,
-0.707917883896095));
#10612=CARTESIAN_POINT('Ctrl Pts',(-0.707917883896095,-0.246942143572133,
-0.679352081686668));
#10613=CARTESIAN_POINT('Ctrl Pts',(-0.722929908501543,-0.244251601209411,
-0.663382628119203));
#10614=CARTESIAN_POINT('Ctrl Pts',(-0.750785745543687,-0.232861760990032,
-0.631684198665439));
#10615=CARTESIAN_POINT('Ctrl Pts',(-0.763642258217232,-0.224161999508995,
-0.615966552324775));
#10616=CARTESIAN_POINT('Ctrl Pts',(-0.78555112003688,-0.203463743702801,
-0.587792702767295));
#10617=CARTESIAN_POINT('Ctrl Pts',(-0.795684265985088,-0.190326085855194,
-0.573915184558107));
#10618=CARTESIAN_POINT('Ctrl Pts',(-0.813159949759,-0.15976606450048,-0.548874290046456));
#10619=CARTESIAN_POINT('Ctrl Pts',(-0.820511285096538,-0.142345102874864,
-0.537715343527944));
#10620=CARTESIAN_POINT('Ctrl Pts',(-0.833661031856294,-0.0999305678883311,
-0.517157748491652));
#10621=CARTESIAN_POINT('Ctrl Pts',(-0.838633903678357,-0.0740444353928836,
-0.508899795931835));
#10622=CARTESIAN_POINT('Ctrl Pts',(-0.841298510752801,-0.04763,-0.504455939115715));
#10623=CARTESIAN_POINT('Origin',(-0.707106781186547,-0.04763,-0.707106781186548));
#10624=CARTESIAN_POINT('Origin',(0.,-0.04763,0.));
#10625=CARTESIAN_POINT('',(-0.238183666596899,-0.04763,-0.951592097314));
#10626=CARTESIAN_POINT('Origin',(0.,-0.04763,0.));
#10627=CARTESIAN_POINT('Origin',(5.55111512312578E-17,-0.04763,-1.));
#10628=CARTESIAN_POINT('Origin',(5.55111512312578E-17,0.,-1.));
#10629=CARTESIAN_POINT('',(0.238183666596899,-0.04763,-0.951592097314));
#10630=CARTESIAN_POINT('Ctrl Pts',(0.238183666596899,-0.04763,-0.951592097314));
#10631=CARTESIAN_POINT('Ctrl Pts',(0.233157223576062,-0.0740444353928835,
-0.952850216871763));
#10632=CARTESIAN_POINT('Ctrl Pts',(0.223801617934946,-0.099930567888331,
-0.955173119738174));
#10633=CARTESIAN_POINT('Ctrl Pts',(0.199966927975188,-0.142345102874864,
-0.960411259488514));
#10634=CARTESIAN_POINT('Ctrl Pts',(0.1868781821531,-0.15976606450048,-0.963103647174702));
#10635=CARTESIAN_POINT('Ctrl Pts',(0.15681442133453,-0.190326085855194,
-0.968453058988463));
#10636=CARTESIAN_POINT('Ctrl Pts',(0.139836317888042,-0.203463743702801,
-0.971100730005489));
#10637=CARTESIAN_POINT('Ctrl Pts',(0.104422493053067,-0.224161999508995,
-0.975530745318961));
#10638=CARTESIAN_POINT('Ctrl Pts',(0.0842175114474173,-0.232861760990032,
-0.977553872336861));
#10639=CARTESIAN_POINT('Ctrl Pts',(0.0421062857595698,-0.244251601209411,
-0.980270995488453));
#10640=CARTESIAN_POINT('Ctrl Pts',(0.0201990724523194,-0.246942143572133,
-0.980948));
#10641=CARTESIAN_POINT('Ctrl Pts',(-0.0201990724523193,-0.246942143572133,
-0.980948));
#10642=CARTESIAN_POINT('Ctrl Pts',(-0.0421062857595697,-0.244251601209411,
-0.980270995488453));
#10643=CARTESIAN_POINT('Ctrl Pts',(-0.0842175114474171,-0.232861760990032,
-0.977553872336861));
#10644=CARTESIAN_POINT('Ctrl Pts',(-0.104422493053067,-0.224161999508995,
-0.975530745318961));
#10645=CARTESIAN_POINT('Ctrl Pts',(-0.139836317888042,-0.203463743702801,
-0.971100730005489));
#10646=CARTESIAN_POINT('Ctrl Pts',(-0.15681442133453,-0.190326085855194,
-0.968453058988463));
#10647=CARTESIAN_POINT('Ctrl Pts',(-0.1868781821531,-0.15976606450048,-0.963103647174702));
#10648=CARTESIAN_POINT('Ctrl Pts',(-0.199966927975188,-0.142345102874864,
-0.960411259488514));
#10649=CARTESIAN_POINT('Ctrl Pts',(-0.223801617934945,-0.099930567888331,
-0.955173119738174));
#10650=CARTESIAN_POINT('Ctrl Pts',(-0.233157223576062,-0.0740444353928835,
-0.952850216871763));
#10651=CARTESIAN_POINT('Ctrl Pts',(-0.238183666596899,-0.0476299999999999,
-0.951592097314));
#10652=CARTESIAN_POINT('Origin',(5.55111512312578E-17,-0.04763,-1.));
#10653=CARTESIAN_POINT('Origin',(0.,-0.04763,0.));
#10654=CARTESIAN_POINT('',(0.504455939115715,-0.04763,-0.841298510752802));
#10655=CARTESIAN_POINT('Origin',(0.,-0.04763,0.));
#10656=CARTESIAN_POINT('Origin',(0.707106781186548,-0.04763,-0.707106781186547));
#10657=CARTESIAN_POINT('Origin',(0.707106781186548,0.,-0.707106781186547));
#10658=CARTESIAN_POINT('',(0.841298510752802,-0.04763,-0.504455939115715));
#10659=CARTESIAN_POINT('Ctrl Pts',(0.841298510752802,-0.04763,-0.504455939115715));
#10660=CARTESIAN_POINT('Ctrl Pts',(0.838633903678357,-0.0740444353928835,
-0.508899795931835));
#10661=CARTESIAN_POINT('Ctrl Pts',(0.833661031856294,-0.0999305678883309,
-0.517157748491652));
#10662=CARTESIAN_POINT('Ctrl Pts',(0.820511285096538,-0.142345102874864,
-0.537715343527944));
#10663=CARTESIAN_POINT('Ctrl Pts',(0.813159949759,-0.159766064500479,-0.548874290046456));
#10664=CARTESIAN_POINT('Ctrl Pts',(0.795684265985088,-0.190326085855194,
-0.573915184558107));
#10665=CARTESIAN_POINT('Ctrl Pts',(0.78555112003688,-0.203463743702801,
-0.587792702767295));
#10666=CARTESIAN_POINT('Ctrl Pts',(0.763642258217233,-0.224161999508995,
-0.615966552324775));
#10667=CARTESIAN_POINT('Ctrl Pts',(0.750785745543687,-0.232861760990032,
-0.631684198665438));
#10668=CARTESIAN_POINT('Ctrl Pts',(0.722929908501543,-0.244251601209411,
-0.663382628119203));
#10669=CARTESIAN_POINT('Ctrl Pts',(0.707917883896095,-0.246942143572133,
-0.679352081686668));
#10670=CARTESIAN_POINT('Ctrl Pts',(0.679352081686668,-0.246942143572133,
-0.707917883896095));
#10671=CARTESIAN_POINT('Ctrl Pts',(0.663382628119203,-0.244251601209411,
-0.722929908501543));
#10672=CARTESIAN_POINT('Ctrl Pts',(0.631684198665438,-0.232861760990032,
-0.750785745543687));
#10673=CARTESIAN_POINT('Ctrl Pts',(0.615966552324775,-0.224161999508995,
-0.763642258217232));
#10674=CARTESIAN_POINT('Ctrl Pts',(0.587792702767295,-0.203463743702801,
-0.78555112003688));
#10675=CARTESIAN_POINT('Ctrl Pts',(0.573915184558107,-0.190326085855194,
-0.795684265985088));
#10676=CARTESIAN_POINT('Ctrl Pts',(0.548874290046456,-0.159766064500479,
-0.813159949759));
#10677=CARTESIAN_POINT('Ctrl Pts',(0.537715343527944,-0.142345102874864,
-0.820511285096538));
#10678=CARTESIAN_POINT('Ctrl Pts',(0.517157748491652,-0.099930567888331,
-0.833661031856294));
#10679=CARTESIAN_POINT('Ctrl Pts',(0.508899795931835,-0.0740444353928835,
-0.838633903678357));
#10680=CARTESIAN_POINT('Ctrl Pts',(0.504455939115715,-0.04763,-0.841298510752801));
#10681=CARTESIAN_POINT('Origin',(0.707106781186548,-0.04763,-0.707106781186547));
#10682=CARTESIAN_POINT('Origin',(0.,-0.166705,0.));
#10683=CARTESIAN_POINT('',(-0.980948,-0.28578,1.20131482833E-16));
#10684=CARTESIAN_POINT('Origin',(0.,-0.28578,0.));
#10685=CARTESIAN_POINT('',(-0.980948,-0.166705,1.20131482833E-16));
#10686=CARTESIAN_POINT('',(0.951592097314,-0.04763,0.238183666596899));
#10687=CARTESIAN_POINT('Origin',(0.,-0.04763,0.));
#10688=CARTESIAN_POINT('',(0.951592097314,-0.04763,-0.238183666596899));
#10689=CARTESIAN_POINT('Ctrl Pts',(0.951592097314,-0.04763,0.238183666596899));
#10690=CARTESIAN_POINT('Ctrl Pts',(0.952850216871763,-0.0740444353928835,
0.233157223576062));
#10691=CARTESIAN_POINT('Ctrl Pts',(0.955173119738174,-0.099930567888331,
0.223801617934945));
#10692=CARTESIAN_POINT('Ctrl Pts',(0.960411259488514,-0.142345102874864,
0.199966927975188));
#10693=CARTESIAN_POINT('Ctrl Pts',(0.963103647174702,-0.15976606450048,
0.1868781821531));
#10694=CARTESIAN_POINT('Ctrl Pts',(0.968453058988463,-0.190326085855194,
0.15681442133453));
#10695=CARTESIAN_POINT('Ctrl Pts',(0.971100730005489,-0.203463743702801,
0.139836317888042));
#10696=CARTESIAN_POINT('Ctrl Pts',(0.975530745318961,-0.224161999508995,
0.104422493053067));
#10697=CARTESIAN_POINT('Ctrl Pts',(0.977553872336861,-0.232861760990032,
0.0842175114474172));
#10698=CARTESIAN_POINT('Ctrl Pts',(0.980270995488453,-0.244251601209411,
0.0421062857595697));
#10699=CARTESIAN_POINT('Ctrl Pts',(0.980948,-0.246942143572133,0.0201990724523194));
#10700=CARTESIAN_POINT('Ctrl Pts',(0.980948,-0.246942143572133,-0.0201990724523194));
#10701=CARTESIAN_POINT('Ctrl Pts',(0.980270995488453,-0.244251601209411,
-0.0421062857595697));
#10702=CARTESIAN_POINT('Ctrl Pts',(0.977553872336861,-0.232861760990032,
-0.0842175114474172));
#10703=CARTESIAN_POINT('Ctrl Pts',(0.975530745318961,-0.224161999508995,
-0.104422493053067));
#10704=CARTESIAN_POINT('Ctrl Pts',(0.971100730005489,-0.203463743702801,
-0.139836317888042));
#10705=CARTESIAN_POINT('Ctrl Pts',(0.968453058988463,-0.190326085855194,
-0.15681442133453));
#10706=CARTESIAN_POINT('Ctrl Pts',(0.963103647174702,-0.15976606450048,
-0.1868781821531));
#10707=CARTESIAN_POINT('Ctrl Pts',(0.960411259488514,-0.142345102874864,
-0.199966927975188));
#10708=CARTESIAN_POINT('Ctrl Pts',(0.955173119738174,-0.099930567888331,
-0.223801617934945));
#10709=CARTESIAN_POINT('Ctrl Pts',(0.952850216871763,-0.0740444353928835,
-0.233157223576062));
#10710=CARTESIAN_POINT('Ctrl Pts',(0.951592097314,-0.0476299999999999,-0.238183666596899));
#10711=CARTESIAN_POINT('Origin',(0.,-0.04763,0.));
#10712=CARTESIAN_POINT('Origin',(0.,-0.04763,0.));
#10713=CARTESIAN_POINT('Origin',(1.,-0.04763,0.));
#10714=CARTESIAN_POINT('Origin',(1.,0.,0.));
#10715=CARTESIAN_POINT('Origin',(1.,-0.04763,0.));
#10716=CARTESIAN_POINT('Origin',(0.,-0.28578,0.));
#10717=CARTESIAN_POINT('Origin',(0.,-0.04763,0.));
#10718=CARTESIAN_POINT('',(0.,0.,0.));
#10719=CARTESIAN_POINT('Origin',(1.013815,0.445,0.));
#10720=CARTESIAN_POINT('',(-1.013815,0.445,-1.24156529467757E-16));
#10721=CARTESIAN_POINT('Origin',(0.,0.445,0.));
#10722=CARTESIAN_POINT('',(-0.991185,0.445,-1.21385153761287E-16));
#10723=CARTESIAN_POINT('Origin',(0.,0.445,0.));
#10724=CARTESIAN_POINT('Origin',(0.,0.4075,0.));
#10725=CARTESIAN_POINT('',(-1.013815,0.37,-1.24156529467757E-16));
#10726=CARTESIAN_POINT('Origin',(0.,0.37,0.));
#10727=CARTESIAN_POINT('',(-1.013815,0.4075,-1.24156529467757E-16));
#10728=CARTESIAN_POINT('Origin',(0.991185,0.37,0.));
#10729=CARTESIAN_POINT('',(-0.991185,0.37,-1.21385153761287E-16));
#10730=CARTESIAN_POINT('Origin',(0.,0.37,0.));
#10731=CARTESIAN_POINT('Origin',(0.,0.4075,0.));
#10732=CARTESIAN_POINT('',(-0.991185,0.4075,-1.21385153761287E-16));
#10733=CARTESIAN_POINT('Origin',(1.013815,-0.37,0.));
#10734=CARTESIAN_POINT('',(-1.013815,-0.37,-1.24156529467757E-16));
#10735=CARTESIAN_POINT('Origin',(0.,-0.37,0.));
#10736=CARTESIAN_POINT('',(-0.991185,-0.37,-1.21385153761287E-16));
#10737=CARTESIAN_POINT('Origin',(0.,-0.37,0.));
#10738=CARTESIAN_POINT('Origin',(0.,-0.4075,0.));
#10739=CARTESIAN_POINT('',(-1.013815,-0.445,-1.24156529467757E-16));
#10740=CARTESIAN_POINT('Origin',(0.,-0.445,0.));
#10741=CARTESIAN_POINT('',(-1.013815,-0.4075,-1.24156529467757E-16));
#10742=CARTESIAN_POINT('Origin',(0.991185,-0.445,0.));
#10743=CARTESIAN_POINT('',(-0.991185,-0.445,-1.21385153761287E-16));
#10744=CARTESIAN_POINT('Origin',(0.,-0.445,0.));
#10745=CARTESIAN_POINT('Origin',(0.,-0.4075,0.));
#10746=CARTESIAN_POINT('',(-0.991185,-0.4075,-1.21385153761287E-16));
#10747=CARTESIAN_POINT('',(0.,0.,0.));
#10748=CARTESIAN_POINT('',(0.,0.,0.));
#10749=CARTESIAN_POINT('',(0.,0.,0.));
#10750=CARTESIAN_POINT('',(0.,0.,0.));
#10751=CARTESIAN_POINT('',(0.,0.,0.));
#10752=CARTESIAN_POINT('',(0.,0.,0.));
#10753=CARTESIAN_POINT('',(0.,0.,0.));
#10754=CARTESIAN_POINT('Origin',(0.,0.,6.9));
#10755=CARTESIAN_POINT('',(-0.165,-2.02066721859313E-17,6.9));
#10756=CARTESIAN_POINT('Origin',(0.,0.,6.9));
#10757=CARTESIAN_POINT('',(-0.165,2.02066721859313E-17,8.));
#10758=CARTESIAN_POINT('',(-0.165,-2.02066721859313E-17,6.9));
#10759=CARTESIAN_POINT('Origin',(0.,0.,8.));
#10760=CARTESIAN_POINT('Origin',(0.,0.,6.9));
#10761=CARTESIAN_POINT('Origin',(-0.429855350392604,2.61349944954989,6.1));
#10762=CARTESIAN_POINT('',(-0.734855350392604,2.61349944954989,6.2));
#10763=CARTESIAN_POINT('Origin',(-0.429855350392604,2.61349944954989,6.2));
#10764=CARTESIAN_POINT('',(-0.734855350392604,2.61349944954989,7.));
#10765=CARTESIAN_POINT('',(-0.734855350392604,2.61349944954989,6.1));
#10766=CARTESIAN_POINT('Origin',(-0.429855350392604,2.61349944954989,7.));
#10767=CARTESIAN_POINT('Origin',(-0.429855350392604,2.61349944954989,6.2));
#10768=CARTESIAN_POINT('',(0.143023559435341,2.21124361718155,6.2));
#10769=CARTESIAN_POINT('',(0.143023559435341,2.21124361718155,7.));
#10770=CARTESIAN_POINT('',(0.143023559435341,2.21124361718155,6.2));
#10771=CARTESIAN_POINT('',(-0.843718811964994,2.04894915491236,6.2));
#10772=CARTESIAN_POINT('Origin',(-0.429855350392604,2.61349944954989,6.2));
#10773=CARTESIAN_POINT('',(-0.843718811964994,2.04894915491236,7.));
#10774=CARTESIAN_POINT('',(-0.843718811964994,2.04894915491236,6.2));
#10775=CARTESIAN_POINT('Origin',(-0.429855350392604,2.61349944954989,7.));
#10776=CARTESIAN_POINT('Origin',(0.493371185700167,0.0811472311345947,6.2));
#10777=CARTESIAN_POINT('',(0.352820058481515,0.935691191757783,7.));
#10778=CARTESIAN_POINT('',(0.0635158353075629,2.69464668068448,7.));
#10779=CARTESIAN_POINT('',(0.352820058481515,0.935691191757783,6.2));
#10780=CARTESIAN_POINT('',(0.352820058481515,0.935691191757783,6.2));
#10781=CARTESIAN_POINT('',(0.0635158353075629,2.69464668068448,6.2));
#10782=CARTESIAN_POINT('Origin',(0.,0.,7.));
#10783=CARTESIAN_POINT('',(-0.63392231291882,0.773396729488594,7.));
#10784=CARTESIAN_POINT('',(-0.493371185700167,-0.0811472311345944,7.));
#10785=CARTESIAN_POINT('Origin',(0.,0.,7.));
#10786=CARTESIAN_POINT('',(-0.5,-6.12323399573677E-17,7.));
#10787=CARTESIAN_POINT('Origin',(0.,0.,7.));
#10788=CARTESIAN_POINT('Origin',(-0.923226536092771,2.53235221841529,6.2));
#10789=CARTESIAN_POINT('',(-0.63392231291882,0.773396729488594,6.2));
#10790=CARTESIAN_POINT('',(-0.493371185700167,-0.0811472311345944,6.2));
#10791=CARTESIAN_POINT('',(-0.63392231291882,0.773396729488594,6.2));
#10792=CARTESIAN_POINT('Origin',(0.,0.,6.2));
#10793=CARTESIAN_POINT('Origin',(0.,0.,6.2));
#10794=CARTESIAN_POINT('Origin',(0.,0.,6.2));
#10795=CARTESIAN_POINT('',(-0.7,-8.57252759403147E-17,6.2));
#10796=CARTESIAN_POINT('Origin',(0.,0.,6.2));
#10797=CARTESIAN_POINT('Origin',(0.,0.,4.95));
#10798=CARTESIAN_POINT('',(-0.7,-8.57252759403147E-17,4.95));
#10799=CARTESIAN_POINT('Origin',(0.,0.,4.95));
#10800=CARTESIAN_POINT('',(-0.5,6.12323399573677E-17,4.95));
#10801=CARTESIAN_POINT('Origin',(0.,0.,4.95));
#10802=CARTESIAN_POINT('Origin',(0.,0.,4.95));
#10803=CARTESIAN_POINT('',(-0.7,-8.57252759403147E-17,4.95));
#10804=CARTESIAN_POINT('Origin',(0.,0.,1.));
#10805=CARTESIAN_POINT('',(-0.5,-6.12323399573677E-17,1.));
#10806=CARTESIAN_POINT('',(-0.5,-6.12323399573677E-17,1.));
#10807=CARTESIAN_POINT('Origin',(0.,0.,1.));
#10808=CARTESIAN_POINT('Origin',(0.,0.,1.));
#10809=CARTESIAN_POINT('',(-0.5,-6.12323399573677E-17,8.));
#10810=CARTESIAN_POINT('Origin',(0.,0.,8.));
#10811=CARTESIAN_POINT('',(-0.5,-6.12323399573677E-17,1.));
#10812=CARTESIAN_POINT('Origin',(0.,0.,8.));
#10813=CARTESIAN_POINT('Origin',(0.,0.,1.));
#10814=CARTESIAN_POINT('',(0.,0.,0.));
#10815=CARTESIAN_POINT('Origin',(0.,0.,1.8));
#10816=CARTESIAN_POINT('',(-0.505,-6.18446633569413E-17,2.05));
#10817=CARTESIAN_POINT('Origin',(0.,0.,2.05));
#10818=CARTESIAN_POINT('',(-0.505,-6.18446633569413E-17,1.8));
#10819=CARTESIAN_POINT('',(-0.505,-6.18446633569413E-17,1.8));
#10820=CARTESIAN_POINT('Origin',(0.,0.,1.8));
#10821=CARTESIAN_POINT('Origin',(0.,0.,1.8));
#10822=CARTESIAN_POINT('',(-0.7,-8.57252759403147E-17,2.05));
#10823=CARTESIAN_POINT('Origin',(0.,0.,2.05));
#10824=CARTESIAN_POINT('',(-0.7,-8.57252759403147E-17,1.8));
#10825=CARTESIAN_POINT('',(-0.7,-8.57252759403147E-17,1.8));
#10826=CARTESIAN_POINT('Origin',(0.,0.,1.8));
#10827=CARTESIAN_POINT('Origin',(0.,0.,2.05));
#10828=CARTESIAN_POINT('Origin',(0.,0.,1.8));
#10829=CARTESIAN_POINT('',(0.,0.,0.));
#10830=CARTESIAN_POINT('Origin',(0.,0.,2.95));
#10831=CARTESIAN_POINT('',(-0.505,-6.18446633569413E-17,4.05));
#10832=CARTESIAN_POINT('Origin',(0.,0.,4.05));
#10833=CARTESIAN_POINT('',(-0.505,-6.18446633569413E-17,2.95));
#10834=CARTESIAN_POINT('',(-0.505,-6.18446633569413E-17,2.95));
#10835=CARTESIAN_POINT('Origin',(0.,0.,2.95));
#10836=CARTESIAN_POINT('Origin',(0.,0.,2.95));
#10837=CARTESIAN_POINT('',(-0.7,-8.57252759403147E-17,4.05));
#10838=CARTESIAN_POINT('Origin',(0.,0.,4.05));
#10839=CARTESIAN_POINT('',(-0.7,-8.57252759403147E-17,2.95));
#10840=CARTESIAN_POINT('',(-0.7,-8.57252759403147E-17,2.95));
#10841=CARTESIAN_POINT('Origin',(0.,0.,2.95));
#10842=CARTESIAN_POINT('Origin',(0.,0.,4.05));
#10843=CARTESIAN_POINT('Origin',(0.,0.,2.95));
#10844=CARTESIAN_POINT('',(0.,0.,0.));
#10845=CARTESIAN_POINT('Origin',(0.49,0.,1.4));
#10846=CARTESIAN_POINT('',(0.49,0.122167917228706,1.28909463493591));
#10847=CARTESIAN_POINT('',(0.49,0.122167917228706,1.51090536506409));
#10848=CARTESIAN_POINT('',(0.49,0.122167917228706,1.));
#10849=CARTESIAN_POINT('Origin',(0.49,0.,1.4));
#10850=CARTESIAN_POINT('Origin',(0.49,0.,1.4));
#10851=CARTESIAN_POINT('',(0.49,-0.122167917228706,1.28909463493591));
#10852=CARTESIAN_POINT('Ctrl Pts',(0.49,-0.122167917228706,1.28909463493591));
#10853=CARTESIAN_POINT('Ctrl Pts',(0.490448531679987,-0.120368913626296,
1.28711294069536));
#10854=CARTESIAN_POINT('Ctrl Pts',(0.490895245371685,-0.118534896565231,
1.28518965877367));
#10855=CARTESIAN_POINT('Ctrl Pts',(0.494795015531646,-0.102111993019358,
1.2687667552278));
#10856=CARTESIAN_POINT('Ctrl Pts',(0.498442514607594,-0.0836597150224318,
1.25609154388858));
#10857=CARTESIAN_POINT('Ctrl Pts',(0.50357781976106,-0.0430495960471595,
1.23920409039234));
#10858=CARTESIAN_POINT('Ctrl Pts',(0.505,-0.020880094330741,1.235));
#10859=CARTESIAN_POINT('Ctrl Pts',(0.505,0.020880094330741,1.235));
#10860=CARTESIAN_POINT('Ctrl Pts',(0.50357781976106,0.0430495960471595,
1.23920409039234));
#10861=CARTESIAN_POINT('Ctrl Pts',(0.498442514607594,0.0836597150224318,
1.25609154388858));
#10862=CARTESIAN_POINT('Ctrl Pts',(0.494795015531646,0.102111993019358,
1.2687667552278));
#10863=CARTESIAN_POINT('Ctrl Pts',(0.490895245371684,0.118534896565231,
1.28518965877367));
#10864=CARTESIAN_POINT('Ctrl Pts',(0.490448531679987,0.120368913626296,
1.28711294069536));
#10865=CARTESIAN_POINT('Ctrl Pts',(0.49,0.122167917228706,1.28909463493591));
#10866=CARTESIAN_POINT('',(0.49,-0.122167917228706,1.51090536506409));
#10867=CARTESIAN_POINT('Origin',(0.49,0.,1.4));
#10868=CARTESIAN_POINT('',(0.505,-1.70422299968729E-17,1.565));
#10869=CARTESIAN_POINT('Ctrl Pts',(0.505,-6.93889390390723E-18,1.565));
#10870=CARTESIAN_POINT('Ctrl Pts',(0.505,-0.020880094330741,1.565));
#10871=CARTESIAN_POINT('Ctrl Pts',(0.50357781976106,-0.0430495960471595,
1.56079590960766));
#10872=CARTESIAN_POINT('Ctrl Pts',(0.498442514607594,-0.0836597150224318,
1.54390845611142));
#10873=CARTESIAN_POINT('Ctrl Pts',(0.494795015531646,-0.102111993019358,
1.5312332447722));
#10874=CARTESIAN_POINT('Ctrl Pts',(0.490895245371684,-0.118534896565231,
1.51481034122633));
#10875=CARTESIAN_POINT('Ctrl Pts',(0.490448531679987,-0.120368913626296,
1.51288705930464));
#10876=CARTESIAN_POINT('Ctrl Pts',(0.49,-0.122167917228706,1.51090536506409));
#10877=CARTESIAN_POINT('',(0.9,-2.02066721859313E-17,1.565));
#10878=CARTESIAN_POINT('',(0.49,-2.02066721859313E-17,1.565));
#10879=CARTESIAN_POINT('',(0.884745726183518,0.165,1.4));
#10880=CARTESIAN_POINT('Ctrl Pts',(0.884745726183518,0.165,1.4));
#10881=CARTESIAN_POINT('Ctrl Pts',(0.884745726183518,0.165,1.37923124059256));
#10882=CARTESIAN_POINT('Ctrl Pts',(0.885552759505264,0.160839719007584,
1.35711110492666));
#10883=CARTESIAN_POINT('Ctrl Pts',(0.888448648150043,0.143986470216691,
1.31647293736623));
#10884=CARTESIAN_POINT('Ctrl Pts',(0.890493604851638,0.131295993814186,
1.29795075602263));
#10885=CARTESIAN_POINT('Ctrl Pts',(0.89431723432394,0.102049819008125,1.26870458121656));
#10886=CARTESIAN_POINT('Ctrl Pts',(0.896347088899543,0.0835273920906824,
1.25601365401642));
#10887=CARTESIAN_POINT('Ctrl Pts',(0.899208271860583,0.0428883760934127,
1.23916007816136));
#10888=CARTESIAN_POINT('Ctrl Pts',(0.9,0.0207679427235068,1.235));
#10889=CARTESIAN_POINT('Ctrl Pts',(0.9,-0.0207679427235068,1.235));
#10890=CARTESIAN_POINT('Ctrl Pts',(0.899208271860583,-0.0428883760934127,
1.23916007816136));
#10891=CARTESIAN_POINT('Ctrl Pts',(0.896347088899543,-0.0835273920906823,
1.25601365401642));
#10892=CARTESIAN_POINT('Ctrl Pts',(0.89431723432394,-0.102049819008125,
1.26870458121656));
#10893=CARTESIAN_POINT('Ctrl Pts',(0.890493604851638,-0.131295993814186,
1.29795075602263));
#10894=CARTESIAN_POINT('Ctrl Pts',(0.888448648150043,-0.143986470216691,
1.31647293736623));
#10895=CARTESIAN_POINT('Ctrl Pts',(0.885552759505264,-0.160839719007584,
1.35711110492666));
#10896=CARTESIAN_POINT('Ctrl Pts',(0.884745726183518,-0.165,1.37923124059256));
#10897=CARTESIAN_POINT('Ctrl Pts',(0.884745726183518,-0.165,1.42076875940744));
#10898=CARTESIAN_POINT('Ctrl Pts',(0.885552759505264,-0.160839719007584,
1.44288889507334));
#10899=CARTESIAN_POINT('Ctrl Pts',(0.888448648150043,-0.14398647021669,
1.48352706263377));
#10900=CARTESIAN_POINT('Ctrl Pts',(0.890493604851638,-0.131295993814186,
1.50204924397737));
#10901=CARTESIAN_POINT('Ctrl Pts',(0.89431723432394,-0.102049819008125,
1.53129541878344));
#10902=CARTESIAN_POINT('Ctrl Pts',(0.896347088899543,-0.0835273920906824,
1.54398634598358));
#10903=CARTESIAN_POINT('Ctrl Pts',(0.899208271860583,-0.0428883760934128,
1.56083992183864));
#10904=CARTESIAN_POINT('Ctrl Pts',(0.9,-0.0207679427235068,1.565));
#10905=CARTESIAN_POINT('Ctrl Pts',(0.9,-6.93889390390723E-18,1.565));
#10906=CARTESIAN_POINT('Ctrl Pts',(0.9,-3.46944695195361E-17,1.565));
#10907=CARTESIAN_POINT('Ctrl Pts',(0.9,0.0207679427235068,1.565));
#10908=CARTESIAN_POINT('Ctrl Pts',(0.899208271860583,0.0428883760934127,
1.56083992183864));
#10909=CARTESIAN_POINT('Ctrl Pts',(0.896347088899543,0.0835273920906824,
1.54398634598358));
#10910=CARTESIAN_POINT('Ctrl Pts',(0.89431723432394,0.102049819008125,1.53129541878344));
#10911=CARTESIAN_POINT('Ctrl Pts',(0.890493604851638,0.131295993814186,
1.50204924397737));
#10912=CARTESIAN_POINT('Ctrl Pts',(0.888448648150043,0.143986470216691,
1.48352706263377));
#10913=CARTESIAN_POINT('Ctrl Pts',(0.885552759505264,0.160839719007584,
1.44288889507334));
#10914=CARTESIAN_POINT('Ctrl Pts',(0.884745726183518,0.165,1.42076875940744));
#10915=CARTESIAN_POINT('Ctrl Pts',(0.884745726183518,0.165,1.4));
#10916=CARTESIAN_POINT('Ctrl Pts',(0.49,0.122167917228706,1.51090536506409));
#10917=CARTESIAN_POINT('Ctrl Pts',(0.490448531679987,0.120368913626296,
1.51288705930464));
#10918=CARTESIAN_POINT('Ctrl Pts',(0.490895245371685,0.118534896565231,
1.51481034122633));
#10919=CARTESIAN_POINT('Ctrl Pts',(0.494795015531646,0.102111993019358,
1.5312332447722));
#10920=CARTESIAN_POINT('Ctrl Pts',(0.498442514607594,0.0836597150224318,
1.54390845611142));
#10921=CARTESIAN_POINT('Ctrl Pts',(0.50357781976106,0.0430495960471594,
1.56079590960766));
#10922=CARTESIAN_POINT('Ctrl Pts',(0.505,0.020880094330741,1.565));
#10923=CARTESIAN_POINT('Ctrl Pts',(0.505,0.,1.565));
#10924=CARTESIAN_POINT('Origin',(0.49,0.,1.4));
#10925=CARTESIAN_POINT('',(0.49,-0.122167917228706,1.));
#10926=CARTESIAN_POINT('Origin',(0.,0.,1.));
#10927=CARTESIAN_POINT('',(-0.505,-6.18446633569413E-17,1.8));
#10928=CARTESIAN_POINT('Origin',(0.,0.,1.8));
#10929=CARTESIAN_POINT('',(-0.505,-6.18446633569413E-17,1.));
#10930=CARTESIAN_POINT('',(-0.505,-6.18446633569413E-17,1.));
#10931=CARTESIAN_POINT('Origin',(0.,0.,1.));
#10932=CARTESIAN_POINT('Origin',(0.,0.,1.));
#10933=CARTESIAN_POINT('',(-0.9,-1.10218211923262E-16,1.8));
#10934=CARTESIAN_POINT('Origin',(0.,0.,1.8));
#10935=CARTESIAN_POINT('',(-0.9,-1.10218211923262E-16,1.));
#10936=CARTESIAN_POINT('',(-0.9,-1.10218211923262E-16,1.));
#10937=CARTESIAN_POINT('Origin',(0.,0.,1.));
#10938=CARTESIAN_POINT('Origin',(0.,0.,1.8));
#10939=CARTESIAN_POINT('Origin',(0.,0.,1.));
#10940=CARTESIAN_POINT('',(0.,0.,0.));
#10941=CARTESIAN_POINT('Origin',(0.49,0.,7.5));
#10942=CARTESIAN_POINT('',(0.49,0.0994987437106618,7.36837553418912));
#10943=CARTESIAN_POINT('',(0.49,0.0994987437106618,7.63162446581088));
#10944=CARTESIAN_POINT('',(0.49,0.0994987437106618,7.));
#10945=CARTESIAN_POINT('Origin',(0.49,0.,7.5));
#10946=CARTESIAN_POINT('Origin',(0.49,0.,7.5));
#10947=CARTESIAN_POINT('',(0.49,-0.0994987437106618,7.36837553418912));
#10948=CARTESIAN_POINT('Ctrl Pts',(0.49,-0.0994987437106616,7.36837553418912));
#10949=CARTESIAN_POINT('Ctrl Pts',(0.492216618113534,-0.0885825970828194,
7.36012370297415));
#10950=CARTESIAN_POINT('Ctrl Pts',(0.4943120869024,-0.0763322372136367,
7.35304490097489));
#10951=CARTESIAN_POINT('Ctrl Pts',(0.498563258730391,-0.0430544276449475,
7.33920540953364));
#10952=CARTESIAN_POINT('Ctrl Pts',(0.5,-0.0208834481936244,7.335));
#10953=CARTESIAN_POINT('Ctrl Pts',(0.5,0.0208834481936244,7.335));
#10954=CARTESIAN_POINT('Ctrl Pts',(0.498563258730391,0.0430544276449475,
7.33920540953364));
#10955=CARTESIAN_POINT('Ctrl Pts',(0.4943120869024,0.0763322372136367,7.3530449009749));
#10956=CARTESIAN_POINT('Ctrl Pts',(0.492216618113534,0.0885825970828194,
7.36012370297415));
#10957=CARTESIAN_POINT('Ctrl Pts',(0.49,0.0994987437106616,7.36837553418912));
#10958=CARTESIAN_POINT('',(0.49,-0.0994987437106618,7.63162446581088));
#10959=CARTESIAN_POINT('Origin',(0.49,0.,7.5));
#10960=CARTESIAN_POINT('',(0.5,3.77445171484879E-18,7.665));
#10961=CARTESIAN_POINT('Ctrl Pts',(0.5,-3.46944695195361E-18,7.665));
#10962=CARTESIAN_POINT('Ctrl Pts',(0.5,-0.0208834481936244,7.665));
#10963=CARTESIAN_POINT('Ctrl Pts',(0.498563258730391,-0.0430544276449474,
7.66079459046636));
#10964=CARTESIAN_POINT('Ctrl Pts',(0.4943120869024,-0.0763322372136367,
7.6469550990251));
#10965=CARTESIAN_POINT('Ctrl Pts',(0.492216618113534,-0.0885825970828193,
7.63987629702585));
#10966=CARTESIAN_POINT('Ctrl Pts',(0.49,-0.0994987437106615,7.63162446581088));
#10967=CARTESIAN_POINT('',(1.2,-2.02066721859313E-17,7.665));
#10968=CARTESIAN_POINT('',(0.49,-2.02066721859313E-17,7.665));
#10969=CARTESIAN_POINT('',(1.18860212013945,0.165,7.5));
#10970=CARTESIAN_POINT('Ctrl Pts',(1.18860212013945,0.165,7.5));
#10971=CARTESIAN_POINT('Ctrl Pts',(1.18860212013945,0.165,7.47925385633929));
#10972=CARTESIAN_POINT('Ctrl Pts',(1.18920136323583,0.16084848971883,7.45714308297918));
#10973=CARTESIAN_POINT('Ctrl Pts',(1.19135875380323,0.144001521209443,7.41649841577523));
#10974=CARTESIAN_POINT('Ctrl Pts',(1.19288497691659,0.131307482946399,7.39796224515484));
#10975=CARTESIAN_POINT('Ctrl Pts',(1.19574431960517,0.102037934403069,7.36869269661151));
#10976=CARTESIAN_POINT('Ctrl Pts',(1.1972642227448,0.0835016860163227,7.35599851755459));
#10977=CARTESIAN_POINT('Ctrl Pts',(1.19940712405299,0.0428567542973023,
7.33915144626121));
#10978=CARTESIAN_POINT('Ctrl Pts',(1.2,0.0207458891223615,7.335));
#10979=CARTESIAN_POINT('Ctrl Pts',(1.2,-0.0207458891223615,7.335));
#10980=CARTESIAN_POINT('Ctrl Pts',(1.19940712405299,-0.0428567542973023,
7.33915144626121));
#10981=CARTESIAN_POINT('Ctrl Pts',(1.1972642227448,-0.0835016860163228,
7.35599851755459));
#10982=CARTESIAN_POINT('Ctrl Pts',(1.19574431960517,-0.102037934403069,
7.36869269661151));
#10983=CARTESIAN_POINT('Ctrl Pts',(1.19288497691659,-0.131307482946399,
7.39796224515484));
#10984=CARTESIAN_POINT('Ctrl Pts',(1.19135875380323,-0.144001521209443,
7.41649841577523));
#10985=CARTESIAN_POINT('Ctrl Pts',(1.18920136323583,-0.16084848971883,7.45714308297918));
#10986=CARTESIAN_POINT('Ctrl Pts',(1.18860212013945,-0.165,7.47925385633929));
#10987=CARTESIAN_POINT('Ctrl Pts',(1.18860212013945,-0.165,7.52074614366071));
#10988=CARTESIAN_POINT('Ctrl Pts',(1.18920136323583,-0.16084848971883,7.54285691702082));
#10989=CARTESIAN_POINT('Ctrl Pts',(1.19135875380323,-0.144001521209443,
7.58350158422477));
#10990=CARTESIAN_POINT('Ctrl Pts',(1.19288497691659,-0.131307482946399,
7.60203775484516));
#10991=CARTESIAN_POINT('Ctrl Pts',(1.19574431960517,-0.102037934403069,
7.63130730338849));
#10992=CARTESIAN_POINT('Ctrl Pts',(1.1972642227448,-0.0835016860163227,
7.64400148244541));
#10993=CARTESIAN_POINT('Ctrl Pts',(1.19940712405299,-0.0428567542973023,
7.66084855373879));
#10994=CARTESIAN_POINT('Ctrl Pts',(1.2,-0.0207458891223615,7.665));
#10995=CARTESIAN_POINT('Ctrl Pts',(1.2,0.,7.665));
#10996=CARTESIAN_POINT('Ctrl Pts',(1.2,-4.85722573273506E-17,7.665));
#10997=CARTESIAN_POINT('Ctrl Pts',(1.2,0.0207458891223614,7.665));
#10998=CARTESIAN_POINT('Ctrl Pts',(1.19940712405299,0.0428567542973022,
7.66084855373879));
#10999=CARTESIAN_POINT('Ctrl Pts',(1.1972642227448,0.0835016860163227,7.64400148244541));
#11000=CARTESIAN_POINT('Ctrl Pts',(1.19574431960517,0.102037934403069,7.63130730338849));
#11001=CARTESIAN_POINT('Ctrl Pts',(1.19288497691659,0.131307482946399,7.60203775484516));
#11002=CARTESIAN_POINT('Ctrl Pts',(1.19135875380323,0.144001521209443,7.58350158422477));
#11003=CARTESIAN_POINT('Ctrl Pts',(1.18920136323583,0.16084848971883,7.54285691702082));
#11004=CARTESIAN_POINT('Ctrl Pts',(1.18860212013945,0.165,7.52074614366071));
#11005=CARTESIAN_POINT('Ctrl Pts',(1.18860212013945,0.165,7.5));
#11006=CARTESIAN_POINT('Ctrl Pts',(0.49,0.0994987437106614,7.63162446581088));
#11007=CARTESIAN_POINT('Ctrl Pts',(0.492216618113534,0.0885825970828193,
7.63987629702585));
#11008=CARTESIAN_POINT('Ctrl Pts',(0.4943120869024,0.0763322372136366,7.6469550990251));
#11009=CARTESIAN_POINT('Ctrl Pts',(0.498563258730391,0.0430544276449474,
7.66079459046636));
#11010=CARTESIAN_POINT('Ctrl Pts',(0.5,0.0208834481936243,7.665));
#11011=CARTESIAN_POINT('Ctrl Pts',(0.5,-5.55111512312578E-17,7.665));
#11012=CARTESIAN_POINT('Origin',(0.49,0.,7.5));
#11013=CARTESIAN_POINT('',(0.49,-0.0994987437106618,7.));
#11014=CARTESIAN_POINT('Origin',(0.,0.,7.));
#11015=CARTESIAN_POINT('',(-0.5,-6.12323399573677E-17,8.));
#11016=CARTESIAN_POINT('Origin',(0.,0.,8.));
#11017=CARTESIAN_POINT('',(-0.5,-6.12323399573677E-17,7.));
#11018=CARTESIAN_POINT('',(-0.5,-6.12323399573677E-17,7.));
#11019=CARTESIAN_POINT('Origin',(0.,0.,7.));
#11020=CARTESIAN_POINT('Origin',(0.,0.,7.));
#11021=CARTESIAN_POINT('',(-1.2,-1.46957615897682E-16,8.));
#11022=CARTESIAN_POINT('Origin',(0.,0.,8.));
#11023=CARTESIAN_POINT('',(-1.2,-1.46957615897682E-16,7.));
#11024=CARTESIAN_POINT('',(-1.2,-1.46957615897682E-16,7.));
#11025=CARTESIAN_POINT('Origin',(0.,0.,7.));
#11026=CARTESIAN_POINT('Origin',(0.,0.,8.));
#11027=CARTESIAN_POINT('Origin',(0.,0.,7.));
#11028=CARTESIAN_POINT('',(0.,0.,0.));
#11029=CARTESIAN_POINT('Origin',(0.,0.,8.));
#11030=CARTESIAN_POINT('',(-0.225,-2.75545529808154E-17,8.2));
#11031=CARTESIAN_POINT('Origin',(0.,0.,8.2));
#11032=CARTESIAN_POINT('',(-0.225,-2.75545529808154E-17,8.));
#11033=CARTESIAN_POINT('',(-0.225,-2.75545529808154E-17,8.));
#11034=CARTESIAN_POINT('Origin',(0.,0.,8.));
#11035=CARTESIAN_POINT('Origin',(0.,0.,8.));
#11036=CARTESIAN_POINT('',(-0.8,-9.79717439317883E-17,8.2));
#11037=CARTESIAN_POINT('Origin',(0.,0.,8.2));
#11038=CARTESIAN_POINT('',(-0.8,-9.79717439317883E-17,8.));
#11039=CARTESIAN_POINT('',(-0.8,-9.79717439317883E-17,8.));
#11040=CARTESIAN_POINT('Origin',(0.,0.,8.));
#11041=CARTESIAN_POINT('Origin',(0.,0.,8.2));
#11042=CARTESIAN_POINT('Origin',(0.,0.,8.));
#11043=CARTESIAN_POINT('',(0.,0.,0.));
#11044=CARTESIAN_POINT('Origin',(-0.429855350392604,2.61349944954989,8.7));
#11045=CARTESIAN_POINT('',(-0.594855350392604,2.61349944954989,8.7));
#11046=CARTESIAN_POINT('Origin',(-0.429855350392604,2.61349944954989,8.7));
#11047=CARTESIAN_POINT('',(-0.594855350392604,2.61349944954989,9.6));
#11048=CARTESIAN_POINT('',(-0.594855350392604,2.61349944954989,8.7));
#11049=CARTESIAN_POINT('Origin',(-0.429855350392604,2.61349944954989,9.6));
#11050=CARTESIAN_POINT('Origin',(-0.429855350392604,2.61349944954989,8.7));
#11051=CARTESIAN_POINT('Origin',(-0.429855350392604,2.61349944954989,6.1));
#11052=CARTESIAN_POINT('',(-0.594855350392604,2.61349944954989,6.2));
#11053=CARTESIAN_POINT('Origin',(-0.429855350392604,2.61349944954989,6.2));
#11054=CARTESIAN_POINT('',(-0.594855350392604,2.61349944954989,7.8));
#11055=CARTESIAN_POINT('',(-0.594855350392604,2.61349944954989,6.1));
#11056=CARTESIAN_POINT('Origin',(-0.429855350392604,2.61349944954989,7.8));
#11057=CARTESIAN_POINT('Origin',(-0.429855350392604,2.61349944954989,7.8));
#11058=CARTESIAN_POINT('Origin',(-0.429855350392604,2.61349944954989,7.4));
#11059=CARTESIAN_POINT('',(-1.1298553503926,2.61349944954989,7.4));
#11060=CARTESIAN_POINT('Origin',(-0.429855350392604,2.61349944954989,7.4));
#11061=CARTESIAN_POINT('',(-0.729855350392604,2.61349944954989,7.4));
#11062=CARTESIAN_POINT('Origin',(-0.429855350392604,2.61349944954989,7.4));
#11063=CARTESIAN_POINT('Origin',(-0.429855350392604,2.61349944954989,7.));
#11064=CARTESIAN_POINT('',(-1.1298553503926,2.61349944954989,7.));
#11065=CARTESIAN_POINT('Origin',(-0.429855350392604,2.61349944954989,7.));
#11066=CARTESIAN_POINT('',(-0.729855350392604,2.61349944954989,7.));
#11067=CARTESIAN_POINT('Origin',(-0.429855350392604,2.61349944954989,7.));
#11068=CARTESIAN_POINT('Origin',(-0.429855350392604,2.61349944954989,7.));
#11069=CARTESIAN_POINT('',(-1.1298553503926,2.61349944954989,7.));
#11070=CARTESIAN_POINT('Origin',(-0.429855350392604,2.61349944954989,6.2));
#11071=CARTESIAN_POINT('',(-0.729855350392604,2.61349944954989,6.2));
#11072=CARTESIAN_POINT('',(-0.729855350392604,2.61349944954989,6.2));
#11073=CARTESIAN_POINT('Origin',(-0.429855350392604,2.61349944954989,6.2));
#11074=CARTESIAN_POINT('Origin',(-0.429855350392604,2.61349944954989,6.2));
#11075=CARTESIAN_POINT('',(-0.729855350392604,2.61349944954989,9.6));
#11076=CARTESIAN_POINT('Origin',(-0.429855350392604,2.61349944954989,9.6));
#11077=CARTESIAN_POINT('',(-0.729855350392604,2.61349944954989,6.2));
#11078=CARTESIAN_POINT('Origin',(-0.429855350392604,2.61349944954989,9.6));
#11079=CARTESIAN_POINT('Origin',(-0.429855350392604,2.61349944954989,6.2));
#11080=CARTESIAN_POINT('',(0.,0.,0.));
#11081=CARTESIAN_POINT('Origin',(-0.429855350392604,2.61349944954989,7.4));
#11082=CARTESIAN_POINT('',(-0.734855350392604,2.61349944954989,8.6));
#11083=CARTESIAN_POINT('Origin',(-0.429855350392604,2.61349944954989,8.6));
#11084=CARTESIAN_POINT('',(-0.734855350392604,2.61349944954989,7.4));
#11085=CARTESIAN_POINT('',(-0.734855350392604,2.61349944954989,7.4));
#11086=CARTESIAN_POINT('Origin',(-0.429855350392604,2.61349944954989,7.4));
#11087=CARTESIAN_POINT('Origin',(-0.429855350392604,2.61349944954989,7.4));
#11088=CARTESIAN_POINT('',(-0.929855350392604,2.61349944954989,8.6));
#11089=CARTESIAN_POINT('Origin',(-0.429855350392604,2.61349944954989,8.6));
#11090=CARTESIAN_POINT('',(-0.929855350392604,2.61349944954989,7.4));
#11091=CARTESIAN_POINT('',(-0.929855350392604,2.61349944954989,7.4));
#11092=CARTESIAN_POINT('Origin',(-0.429855350392604,2.61349944954989,7.4));
#11093=CARTESIAN_POINT('Origin',(-0.429855350392604,2.61349944954989,8.6));
#11094=CARTESIAN_POINT('Origin',(-0.429855350392604,2.61349944954989,7.4));
#11095=CARTESIAN_POINT('',(0.,0.,0.));
#11096=CARTESIAN_POINT('Origin',(-0.429855350392604,2.61349944954989,9.4));
#11097=CARTESIAN_POINT('',(-0.734855350392604,2.61349944954989,9.6));
#11098=CARTESIAN_POINT('Origin',(-0.429855350392604,2.61349944954989,9.6));
#11099=CARTESIAN_POINT('',(-0.734855350392604,2.61349944954989,9.4));
#11100=CARTESIAN_POINT('',(-0.734855350392604,2.61349944954989,9.4));
#11101=CARTESIAN_POINT('Origin',(-0.429855350392604,2.61349944954989,9.4));
#11102=CARTESIAN_POINT('Origin',(-0.429855350392604,2.61349944954989,9.4));
#11103=CARTESIAN_POINT('',(-0.929855350392604,2.61349944954989,9.6));
#11104=CARTESIAN_POINT('Origin',(-0.429855350392604,2.61349944954989,9.6));
#11105=CARTESIAN_POINT('',(-0.929855350392604,2.61349944954989,9.4));
#11106=CARTESIAN_POINT('',(-0.929855350392604,2.61349944954989,9.4));
#11107=CARTESIAN_POINT('Origin',(-0.429855350392604,2.61349944954989,9.4));
#11108=CARTESIAN_POINT('Origin',(-0.429855350392604,2.61349944954989,9.6));
#11109=CARTESIAN_POINT('Origin',(-0.429855350392604,2.61349944954989,9.4));
#11110=CARTESIAN_POINT('',(0.,0.,0.));
#11111=CARTESIAN_POINT('Origin',(-0.429855350392604,2.61349944954989,6.));
#11112=CARTESIAN_POINT('',(-0.654855350392604,2.61349944954989,6.2));
#11113=CARTESIAN_POINT('Origin',(-0.429855350392604,2.61349944954989,6.2));
#11114=CARTESIAN_POINT('',(-0.654855350392604,2.61349944954989,6.));
#11115=CARTESIAN_POINT('',(-0.654855350392604,2.61349944954989,6.));
#11116=CARTESIAN_POINT('Origin',(-0.429855350392604,2.61349944954989,6.));
#11117=CARTESIAN_POINT('Origin',(-0.429855350392604,2.61349944954989,6.));
#11118=CARTESIAN_POINT('',(-1.0298553503926,2.61349944954989,6.2));
#11119=CARTESIAN_POINT('Origin',(-0.429855350392604,2.61349944954989,6.2));
#11120=CARTESIAN_POINT('',(-1.0298553503926,2.61349944954989,6.));
#11121=CARTESIAN_POINT('',(-1.0298553503926,2.61349944954989,6.));
#11122=CARTESIAN_POINT('Origin',(-0.429855350392604,2.61349944954989,6.));
#11123=CARTESIAN_POINT('Origin',(-0.429855350392604,2.61349944954989,6.2));
#11124=CARTESIAN_POINT('Origin',(-0.429855350392604,2.61349944954989,6.));
#11125=CARTESIAN_POINT('',(0.,0.,0.));
#11126=CARTESIAN_POINT('Origin',(-0.429855350392604,2.61349944954989,9.6));
#11127=CARTESIAN_POINT('',(-0.654855350392604,2.61349944954989,9.8));
#11128=CARTESIAN_POINT('Origin',(-0.429855350392604,2.61349944954989,9.8));
#11129=CARTESIAN_POINT('',(-0.654855350392604,2.61349944954989,9.6));
#11130=CARTESIAN_POINT('',(-0.654855350392604,2.61349944954989,9.6));
#11131=CARTESIAN_POINT('Origin',(-0.429855350392604,2.61349944954989,9.6));
#11132=CARTESIAN_POINT('Origin',(-0.429855350392604,2.61349944954989,9.6));
#11133=CARTESIAN_POINT('',(-0.929855350392604,2.61349944954989,9.8));
#11134=CARTESIAN_POINT('Origin',(-0.429855350392604,2.61349944954989,9.8));
#11135=CARTESIAN_POINT('',(-0.929855350392604,2.61349944954989,9.6));
#11136=CARTESIAN_POINT('',(-0.929855350392604,2.61349944954989,9.6));
#11137=CARTESIAN_POINT('Origin',(-0.429855350392604,2.61349944954989,9.6));
#11138=CARTESIAN_POINT('Origin',(-0.429855350392604,2.61349944954989,9.8));
#11139=CARTESIAN_POINT('Origin',(-0.429855350392604,2.61349944954989,9.6));
#11140=CARTESIAN_POINT('',(0.,0.,0.));
#11141=CARTESIAN_POINT('Origin',(0.0577350269189626,0.,-0.1));
#11142=CARTESIAN_POINT('',(0.0577350269189626,0.,-0.1));
#11143=CARTESIAN_POINT('',(0.115470053837925,0.,0.));
#11144=CARTESIAN_POINT('',(0.0934187836487032,0.,-0.0381939203391614));
#11145=CARTESIAN_POINT('',(0.0577350269189626,-0.2,-0.1));
#11146=CARTESIAN_POINT('',(0.0577350269189626,0.,-0.1));
#11147=CARTESIAN_POINT('',(0.115470053837925,-0.2,0.));
#11148=CARTESIAN_POINT('',(0.115470053837925,-0.2,0.));
#11149=CARTESIAN_POINT('',(0.115470053837925,0.,0.));
#11150=CARTESIAN_POINT('Origin',(-0.0577350269189626,0.,-0.1));
#11151=CARTESIAN_POINT('',(-0.0577350269189626,0.,-0.1));
#11152=CARTESIAN_POINT('',(0.0561324865405187,0.,-0.1));
#11153=CARTESIAN_POINT('',(-0.0577350269189626,-0.2,-0.1));
#11154=CARTESIAN_POINT('',(-0.0577350269189626,0.,-0.1));
#11155=CARTESIAN_POINT('',(0.0577350269189626,-0.2,-0.1));
#11156=CARTESIAN_POINT('Origin',(-0.115470053837925,0.,-1.38777878078145E-17));
#11157=CARTESIAN_POINT('',(-0.115470053837925,0.,-1.41410031829988E-17));
#11158=CARTESIAN_POINT('',(-0.0797862971081845,0.,-0.0618060796608387));
#11159=CARTESIAN_POINT('',(-0.115470053837925,-0.2,-1.38777878078145E-17));
#11160=CARTESIAN_POINT('',(-0.115470053837925,0.,-1.41410031829988E-17));
#11161=CARTESIAN_POINT('',(-0.0577350269189626,-0.2,-0.1));
#11162=CARTESIAN_POINT('Origin',(-0.0577350269189626,0.,0.1));
#11163=CARTESIAN_POINT('',(-0.0577350269189626,0.,0.1));
#11164=CARTESIAN_POINT('',(-0.0509187836487033,0.,0.111806079660839));
#11165=CARTESIAN_POINT('',(-0.0577350269189626,-0.2,0.1));
#11166=CARTESIAN_POINT('',(-0.0577350269189626,0.,0.1));
#11167=CARTESIAN_POINT('',(-0.115470053837925,-0.2,-1.41410031829988E-17));
#11168=CARTESIAN_POINT('Origin',(0.0577350269189626,0.,0.1));
#11169=CARTESIAN_POINT('',(0.0577350269189626,0.,0.1));
#11170=CARTESIAN_POINT('',(0.113867513459481,0.,0.1));
#11171=CARTESIAN_POINT('',(0.0577350269189626,-0.2,0.1));
#11172=CARTESIAN_POINT('',(0.0577350269189626,0.,0.1));
#11173=CARTESIAN_POINT('',(-0.0577350269189626,-0.2,0.1));
#11174=CARTESIAN_POINT('Origin',(0.115470053837925,0.,0.));
#11175=CARTESIAN_POINT('',(0.122286297108185,0.,-0.0118060796608386));
#11176=CARTESIAN_POINT('',(0.0577350269189626,-0.2,0.1));
#11177=CARTESIAN_POINT('Origin',(0.,-0.2,0.));
#11178=CARTESIAN_POINT('Origin',(0.17,0.,0.));
#11179=CARTESIAN_POINT('',(-0.17,-8.67361737988404E-18,-2.0818995585505E-17));
#11180=CARTESIAN_POINT('Origin',(0.,0.,0.));
#11181=CARTESIAN_POINT('Origin',(0.,-0.015,0.));
#11182=CARTESIAN_POINT('',(-0.1954,-0.0254,-2.39295984553393E-17));
#11183=CARTESIAN_POINT('Origin',(0.,-0.0254,0.));
#11184=CARTESIAN_POINT('',(-0.185,-0.015,-2.2655965784226E-17));
#11185=CARTESIAN_POINT('Origin',(0.,-0.2775,0.));
#11186=CARTESIAN_POINT('',(-0.1954,-0.5296,2.39295984553393E-17));
#11187=CARTESIAN_POINT('Origin',(0.,-0.5296,0.));
#11188=CARTESIAN_POINT('',(-0.1954,-0.2775,-2.39295984553393E-17));
#11189=CARTESIAN_POINT('Origin',(0.,-0.5625,0.));
#11190=CARTESIAN_POINT('',(-0.125,-0.6,-1.53080849893419E-17));
#11191=CARTESIAN_POINT('Origin',(0.,-0.6,0.));
#11192=CARTESIAN_POINT('',(-0.1625,-0.5625,-1.99005104861445E-17));
#11193=CARTESIAN_POINT('Origin',(0.,-0.6,0.));
#11194=CARTESIAN_POINT('',(0.,0.,0.));
#11195=CARTESIAN_POINT('',(0.,0.,0.));
#11196=CARTESIAN_POINT('Origin',(9.5,-1.,12.9));
#11197=CARTESIAN_POINT('',(9.225,-1.,13.));
#11198=CARTESIAN_POINT('Origin',(9.5,-1.,13.));
#11199=CARTESIAN_POINT('',(9.225,-1.,13.8));
#11200=CARTESIAN_POINT('',(9.225,-1.,12.9));
#11201=CARTESIAN_POINT('Origin',(9.5,-1.,13.8));
#11202=CARTESIAN_POINT('Origin',(6.5,1.,12.9));
#11203=CARTESIAN_POINT('',(6.225,1.,13.));
#11204=CARTESIAN_POINT('Origin',(6.5,1.,13.));
#11205=CARTESIAN_POINT('',(6.225,1.,13.8));
#11206=CARTESIAN_POINT('',(6.225,1.,12.9));
#11207=CARTESIAN_POINT('Origin',(6.5,1.,13.8));
#11208=CARTESIAN_POINT('Origin',(6.5,-1.,12.9));
#11209=CARTESIAN_POINT('',(6.225,-1.,13.));
#11210=CARTESIAN_POINT('Origin',(6.5,-1.,13.));
#11211=CARTESIAN_POINT('',(6.225,-1.,13.8));
#11212=CARTESIAN_POINT('',(6.225,-1.,12.9));
#11213=CARTESIAN_POINT('Origin',(6.5,-1.,13.8));
#11214=CARTESIAN_POINT('Origin',(9.5,1.,12.9));
#11215=CARTESIAN_POINT('',(9.225,1.,13.));
#11216=CARTESIAN_POINT('Origin',(9.5,1.,13.));
#11217=CARTESIAN_POINT('',(9.225,1.,13.8));
#11218=CARTESIAN_POINT('',(9.225,1.,12.9));
#11219=CARTESIAN_POINT('Origin',(9.5,1.,13.8));
#11220=CARTESIAN_POINT('Origin',(8.,0.,13.));
#11221=CARTESIAN_POINT('',(6.,1.5,13.));
#11222=CARTESIAN_POINT('',(6.,-1.5,13.));
#11223=CARTESIAN_POINT('',(6.,1.5,13.));
#11224=CARTESIAN_POINT('',(10.,1.5,13.));
#11225=CARTESIAN_POINT('',(10.,1.5,13.));
#11226=CARTESIAN_POINT('',(10.,-1.5,13.));
#11227=CARTESIAN_POINT('',(10.,-1.5,13.));
#11228=CARTESIAN_POINT('',(6.,-1.5,13.));
#11229=CARTESIAN_POINT('',(7.2,-9.79717439317883E-17,13.));
#11230=CARTESIAN_POINT('Origin',(8.,0.,13.));
#11231=CARTESIAN_POINT('Origin',(10.,1.5,13.));
#11232=CARTESIAN_POINT('',(6.,1.5,13.8));
#11233=CARTESIAN_POINT('',(6.,1.5,13.));
#11234=CARTESIAN_POINT('',(10.,1.5,13.8));
#11235=CARTESIAN_POINT('',(10.,1.5,13.8));
#11236=CARTESIAN_POINT('',(10.,1.5,13.));
#11237=CARTESIAN_POINT('Origin',(10.,-1.5,13.));
#11238=CARTESIAN_POINT('',(10.,-1.5,13.8));
#11239=CARTESIAN_POINT('',(10.,-1.5,13.8));
#11240=CARTESIAN_POINT('',(10.,-1.5,13.));
#11241=CARTESIAN_POINT('Origin',(6.,-1.5,13.));
#11242=CARTESIAN_POINT('',(6.,-1.5,13.8));
#11243=CARTESIAN_POINT('',(6.,-1.5,13.8));
#11244=CARTESIAN_POINT('',(6.,-1.5,13.));
#11245=CARTESIAN_POINT('Origin',(6.,1.5,13.));
#11246=CARTESIAN_POINT('',(6.,1.5,13.8));
#11247=CARTESIAN_POINT('Origin',(8.,0.,13.8));
#11248=CARTESIAN_POINT('Origin',(8.,0.,7.));
#11249=CARTESIAN_POINT('',(7.2,-9.79717439317883E-17,7.));
#11250=CARTESIAN_POINT('',(7.2,-9.79717439317883E-17,7.));
#11251=CARTESIAN_POINT('Origin',(8.,0.,7.));
#11252=CARTESIAN_POINT('Origin',(8.,4.,6.1));
#11253=CARTESIAN_POINT('',(7.695,4.,6.2));
#11254=CARTESIAN_POINT('Origin',(8.,4.,6.2));
#11255=CARTESIAN_POINT('',(7.695,4.,7.));
#11256=CARTESIAN_POINT('',(7.695,4.,6.1));
#11257=CARTESIAN_POINT('Origin',(8.,4.,7.));
#11258=CARTESIAN_POINT('Origin',(8.,4.,6.2));
#11259=CARTESIAN_POINT('',(8.5,3.51010205144337,6.2));
#11260=CARTESIAN_POINT('',(8.5,3.51010205144337,7.));
#11261=CARTESIAN_POINT('',(8.5,3.51010205144337,6.2));
#11262=CARTESIAN_POINT('',(7.5,3.51010205144337,6.2));
#11263=CARTESIAN_POINT('Origin',(8.,4.,6.2));
#11264=CARTESIAN_POINT('',(7.5,3.51010205144337,7.));
#11265=CARTESIAN_POINT('',(7.5,3.51010205144337,6.2));
#11266=CARTESIAN_POINT('Origin',(8.,4.,7.));
#11267=CARTESIAN_POINT('Origin',(8.5,0.,6.2));
#11268=CARTESIAN_POINT('',(8.5,0.866025403784439,7.));
#11269=CARTESIAN_POINT('',(8.5,4.,7.));
#11270=CARTESIAN_POINT('',(8.5,0.866025403784439,6.2));
#11271=CARTESIAN_POINT('',(8.5,0.866025403784439,6.2));
#11272=CARTESIAN_POINT('',(8.5,4.,6.2));
#11273=CARTESIAN_POINT('Origin',(8.,0.,7.));
#11274=CARTESIAN_POINT('',(7.5,0.866025403784439,7.));
#11275=CARTESIAN_POINT('',(7.5,0.,7.));
#11276=CARTESIAN_POINT('Origin',(8.,0.,7.));
#11277=CARTESIAN_POINT('Origin',(7.5,4.,6.2));
#11278=CARTESIAN_POINT('',(7.5,0.866025403784439,6.2));
#11279=CARTESIAN_POINT('',(7.5,0.,6.2));
#11280=CARTESIAN_POINT('',(7.5,0.866025403784439,6.2));
#11281=CARTESIAN_POINT('Origin',(8.,0.,6.2));
#11282=CARTESIAN_POINT('Origin',(8.,0.,6.2));
#11283=CARTESIAN_POINT('Origin',(8.,0.,6.2));
#11284=CARTESIAN_POINT('',(7.3,-8.57252759403146E-17,6.2));
#11285=CARTESIAN_POINT('Origin',(8.,0.,6.2));
#11286=CARTESIAN_POINT('Origin',(8.,0.,3.95));
#11287=CARTESIAN_POINT('',(7.3,-8.57252759403146E-17,3.95));
#11288=CARTESIAN_POINT('Origin',(8.,0.,3.95));
#11289=CARTESIAN_POINT('',(7.5,6.12323399573677E-17,3.95));
#11290=CARTESIAN_POINT('Origin',(8.,0.,3.95));
#11291=CARTESIAN_POINT('Origin',(8.,0.,3.95));
#11292=CARTESIAN_POINT('',(7.3,-8.57252759403146E-17,3.95));
#11293=CARTESIAN_POINT('Origin',(8.,0.,1.));
#11294=CARTESIAN_POINT('',(7.5,-6.12323399573677E-17,1.));
#11295=CARTESIAN_POINT('',(7.5,-6.12323399573677E-17,1.));
#11296=CARTESIAN_POINT('Origin',(8.,0.,1.));
#11297=CARTESIAN_POINT('Origin',(8.,0.,1.));
#11298=CARTESIAN_POINT('',(0.,0.,0.));
#11299=CARTESIAN_POINT('Origin',(8.,0.,1.8));
#11300=CARTESIAN_POINT('',(7.495,-6.18446633569414E-17,3.05));
#11301=CARTESIAN_POINT('Origin',(8.,0.,3.05));
#11302=CARTESIAN_POINT('',(7.495,-6.18446633569414E-17,1.8));
#11303=CARTESIAN_POINT('',(7.495,-6.18446633569414E-17,1.8));
#11304=CARTESIAN_POINT('Origin',(8.,0.,1.8));
#11305=CARTESIAN_POINT('Origin',(8.,0.,1.8));
#11306=CARTESIAN_POINT('',(7.3,-8.57252759403146E-17,3.05));
#11307=CARTESIAN_POINT('Origin',(8.,0.,3.05));
#11308=CARTESIAN_POINT('',(7.3,-8.57252759403146E-17,1.8));
#11309=CARTESIAN_POINT('',(7.3,-8.57252759403146E-17,1.8));
#11310=CARTESIAN_POINT('Origin',(8.,0.,1.8));
#11311=CARTESIAN_POINT('Origin',(8.,0.,3.05));
#11312=CARTESIAN_POINT('Origin',(8.,0.,1.8));
#11313=CARTESIAN_POINT('',(0.,0.,0.));
#11314=CARTESIAN_POINT('Origin',(8.49,0.,1.4));
#11315=CARTESIAN_POINT('',(8.49,0.122167917228709,1.28909463493591));
#11316=CARTESIAN_POINT('',(8.49,0.122167917228709,1.51090536506409));
#11317=CARTESIAN_POINT('',(8.49,0.122167917228709,1.));
#11318=CARTESIAN_POINT('Origin',(8.49,0.,1.4));
#11319=CARTESIAN_POINT('Origin',(8.49,0.,1.4));
#11320=CARTESIAN_POINT('',(8.49,-0.122167917228709,1.28909463493591));
#11321=CARTESIAN_POINT('Ctrl Pts',(8.49,-0.122167917228708,1.28909463493591));
#11322=CARTESIAN_POINT('Ctrl Pts',(8.49044853167999,-0.120368913626297,
1.28711294069536));
#11323=CARTESIAN_POINT('Ctrl Pts',(8.49089524537169,-0.118534896565232,
1.28518965877367));
#11324=CARTESIAN_POINT('Ctrl Pts',(8.49479501553165,-0.102111993019358,
1.2687667552278));
#11325=CARTESIAN_POINT('Ctrl Pts',(8.49844251460759,-0.0836597150224316,
1.25609154388858));
#11326=CARTESIAN_POINT('Ctrl Pts',(8.50357781976106,-0.0430495960471594,
1.23920409039234));
#11327=CARTESIAN_POINT('Ctrl Pts',(8.505,-0.020880094330741,1.235));
#11328=CARTESIAN_POINT('Ctrl Pts',(8.505,0.020880094330741,1.235));
#11329=CARTESIAN_POINT('Ctrl Pts',(8.50357781976106,0.0430495960471594,
1.23920409039234));
#11330=CARTESIAN_POINT('Ctrl Pts',(8.49844251460759,0.0836597150224316,
1.25609154388858));
#11331=CARTESIAN_POINT('Ctrl Pts',(8.49479501553165,0.102111993019358,1.2687667552278));
#11332=CARTESIAN_POINT('Ctrl Pts',(8.49089524537169,0.118534896565232,1.28518965877367));
#11333=CARTESIAN_POINT('Ctrl Pts',(8.49044853167999,0.120368913626297,1.28711294069536));
#11334=CARTESIAN_POINT('Ctrl Pts',(8.49,0.122167917228708,1.28909463493591));
#11335=CARTESIAN_POINT('',(8.49,-0.122167917228709,1.51090536506409));
#11336=CARTESIAN_POINT('Origin',(8.49,0.,1.4));
#11337=CARTESIAN_POINT('',(8.505,-2.05116769488265E-17,1.565));
#11338=CARTESIAN_POINT('Ctrl Pts',(8.505,-2.08166817117217E-17,1.565));
#11339=CARTESIAN_POINT('Ctrl Pts',(8.505,-0.020880094330741,1.565));
#11340=CARTESIAN_POINT('Ctrl Pts',(8.50357781976106,-0.0430495960471594,
1.56079590960766));
#11341=CARTESIAN_POINT('Ctrl Pts',(8.49844251460759,-0.0836597150224316,
1.54390845611142));
#11342=CARTESIAN_POINT('Ctrl Pts',(8.49479501553165,-0.102111993019358,
1.5312332447722));
#11343=CARTESIAN_POINT('Ctrl Pts',(8.49089524537169,-0.118534896565232,
1.51481034122633));
#11344=CARTESIAN_POINT('Ctrl Pts',(8.49044853167999,-0.120368913626297,
1.51288705930464));
#11345=CARTESIAN_POINT('Ctrl Pts',(8.49,-0.122167917228708,1.51090536506409));
#11346=CARTESIAN_POINT('',(8.9,-2.02066721859313E-17,1.565));
#11347=CARTESIAN_POINT('',(8.49,-2.02066721859313E-17,1.565));
#11348=CARTESIAN_POINT('',(8.88474572618352,0.165,1.4));
#11349=CARTESIAN_POINT('Ctrl Pts',(8.88474572618352,0.165,1.4));
#11350=CARTESIAN_POINT('Ctrl Pts',(8.88474572618352,0.165,1.37923124059256));
#11351=CARTESIAN_POINT('Ctrl Pts',(8.88555275950526,0.160839719007584,1.35711110492666));
#11352=CARTESIAN_POINT('Ctrl Pts',(8.88844864815004,0.143986470216691,1.31647293736623));
#11353=CARTESIAN_POINT('Ctrl Pts',(8.89049360485164,0.131295993814186,1.29795075602263));
#11354=CARTESIAN_POINT('Ctrl Pts',(8.89431723432394,0.102049819008125,1.26870458121656));
#11355=CARTESIAN_POINT('Ctrl Pts',(8.89634708889954,0.0835273920906824,
1.25601365401642));
#11356=CARTESIAN_POINT('Ctrl Pts',(8.89920827186059,0.0428883760934127,
1.23916007816136));
#11357=CARTESIAN_POINT('Ctrl Pts',(8.9,0.0207679427235068,1.235));
#11358=CARTESIAN_POINT('Ctrl Pts',(8.9,-0.0207679427235068,1.235));
#11359=CARTESIAN_POINT('Ctrl Pts',(8.89920827186059,-0.0428883760934129,
1.23916007816136));
#11360=CARTESIAN_POINT('Ctrl Pts',(8.89634708889954,-0.0835273920906825,
1.25601365401642));
#11361=CARTESIAN_POINT('Ctrl Pts',(8.89431723432394,-0.102049819008125,
1.26870458121656));
#11362=CARTESIAN_POINT('Ctrl Pts',(8.89049360485164,-0.131295993814186,
1.29795075602263));
#11363=CARTESIAN_POINT('Ctrl Pts',(8.88844864815004,-0.143986470216691,
1.31647293736623));
#11364=CARTESIAN_POINT('Ctrl Pts',(8.88555275950526,-0.160839719007584,
1.35711110492666));
#11365=CARTESIAN_POINT('Ctrl Pts',(8.88474572618352,-0.165,1.37923124059256));
#11366=CARTESIAN_POINT('Ctrl Pts',(8.88474572618352,-0.165,1.42076875940744));
#11367=CARTESIAN_POINT('Ctrl Pts',(8.88555275950526,-0.160839719007584,
1.44288889507334));
#11368=CARTESIAN_POINT('Ctrl Pts',(8.88844864815004,-0.143986470216691,
1.48352706263377));
#11369=CARTESIAN_POINT('Ctrl Pts',(8.89049360485164,-0.131295993814186,
1.50204924397737));
#11370=CARTESIAN_POINT('Ctrl Pts',(8.89431723432394,-0.102049819008125,
1.53129541878344));
#11371=CARTESIAN_POINT('Ctrl Pts',(8.89634708889954,-0.0835273920906824,
1.54398634598358));
#11372=CARTESIAN_POINT('Ctrl Pts',(8.89920827186059,-0.0428883760934127,
1.56083992183864));
#11373=CARTESIAN_POINT('Ctrl Pts',(8.9,-0.0207679427235068,1.565));
#11374=CARTESIAN_POINT('Ctrl Pts',(8.9,-2.08166817117217E-17,1.565));
#11375=CARTESIAN_POINT('Ctrl Pts',(8.9,-2.77555756156289E-17,1.565));
#11376=CARTESIAN_POINT('Ctrl Pts',(8.9,0.0207679427235068,1.565));
#11377=CARTESIAN_POINT('Ctrl Pts',(8.89920827186059,0.0428883760934128,
1.56083992183864));
#11378=CARTESIAN_POINT('Ctrl Pts',(8.89634708889954,0.0835273920906824,
1.54398634598358));
#11379=CARTESIAN_POINT('Ctrl Pts',(8.89431723432394,0.102049819008125,1.53129541878344));
#11380=CARTESIAN_POINT('Ctrl Pts',(8.89049360485164,0.131295993814186,1.50204924397737));
#11381=CARTESIAN_POINT('Ctrl Pts',(8.88844864815004,0.143986470216691,1.48352706263377));
#11382=CARTESIAN_POINT('Ctrl Pts',(8.88555275950526,0.160839719007584,1.44288889507334));
#11383=CARTESIAN_POINT('Ctrl Pts',(8.88474572618352,0.165,1.42076875940744));
#11384=CARTESIAN_POINT('Ctrl Pts',(8.88474572618352,0.165,1.4));
#11385=CARTESIAN_POINT('Ctrl Pts',(8.49,0.122167917228708,1.51090536506409));
#11386=CARTESIAN_POINT('Ctrl Pts',(8.49044853167999,0.120368913626297,1.51288705930464));
#11387=CARTESIAN_POINT('Ctrl Pts',(8.49089524537169,0.118534896565232,1.51481034122633));
#11388=CARTESIAN_POINT('Ctrl Pts',(8.49479501553165,0.102111993019358,1.5312332447722));
#11389=CARTESIAN_POINT('Ctrl Pts',(8.49844251460759,0.0836597150224316,
1.54390845611142));
#11390=CARTESIAN_POINT('Ctrl Pts',(8.50357781976106,0.0430495960471594,
1.56079590960766));
#11391=CARTESIAN_POINT('Ctrl Pts',(8.505,0.0208800943307409,1.565));
#11392=CARTESIAN_POINT('Ctrl Pts',(8.505,-6.93889390390723E-17,1.565));
#11393=CARTESIAN_POINT('Origin',(8.49,0.,1.4));
#11394=CARTESIAN_POINT('',(8.49,-0.122167917228709,1.));
#11395=CARTESIAN_POINT('Origin',(8.,0.,1.));
#11396=CARTESIAN_POINT('',(7.495,-6.18446633569414E-17,1.8));
#11397=CARTESIAN_POINT('Origin',(8.,0.,1.8));
#11398=CARTESIAN_POINT('',(7.495,-6.18446633569414E-17,1.));
#11399=CARTESIAN_POINT('',(7.495,-6.18446633569414E-17,1.));
#11400=CARTESIAN_POINT('Origin',(8.,0.,1.));
#11401=CARTESIAN_POINT('Origin',(8.,0.,1.));
#11402=CARTESIAN_POINT('',(7.1,-1.10218211923262E-16,1.8));
#11403=CARTESIAN_POINT('Origin',(8.,0.,1.8));
#11404=CARTESIAN_POINT('',(7.1,-1.10218211923262E-16,1.));
#11405=CARTESIAN_POINT('',(7.1,-1.10218211923262E-16,1.));
#11406=CARTESIAN_POINT('Origin',(8.,0.,1.));
#11407=CARTESIAN_POINT('Origin',(8.,0.,1.8));
#11408=CARTESIAN_POINT('Origin',(8.,0.,1.));
#11409=CARTESIAN_POINT('',(0.,0.,0.));
#11410=CARTESIAN_POINT('Origin',(8.,4.,8.7));
#11411=CARTESIAN_POINT('',(7.835,4.,8.7));
#11412=CARTESIAN_POINT('Origin',(8.,4.,8.7));
#11413=CARTESIAN_POINT('',(7.835,4.,9.6));
#11414=CARTESIAN_POINT('',(7.835,4.,8.7));
#11415=CARTESIAN_POINT('Origin',(8.,4.,9.6));
#11416=CARTESIAN_POINT('Origin',(8.,4.,8.7));
#11417=CARTESIAN_POINT('Origin',(8.,4.,6.1));
#11418=CARTESIAN_POINT('',(7.835,4.,6.2));
#11419=CARTESIAN_POINT('Origin',(8.,4.,6.2));
#11420=CARTESIAN_POINT('',(7.835,4.,7.8));
#11421=CARTESIAN_POINT('',(7.835,4.,6.1));
#11422=CARTESIAN_POINT('Origin',(8.,4.,7.8));
#11423=CARTESIAN_POINT('Origin',(8.,4.,7.8));
#11424=CARTESIAN_POINT('Origin',(8.,4.,7.4));
#11425=CARTESIAN_POINT('',(7.3,4.,7.4));
#11426=CARTESIAN_POINT('Origin',(8.,4.,7.4));
#11427=CARTESIAN_POINT('',(7.7,4.,7.4));
#11428=CARTESIAN_POINT('Origin',(8.,4.,7.4));
#11429=CARTESIAN_POINT('Origin',(8.,4.,7.));
#11430=CARTESIAN_POINT('',(7.3,4.,7.));
#11431=CARTESIAN_POINT('Origin',(8.,4.,7.));
#11432=CARTESIAN_POINT('',(7.7,4.,7.));
#11433=CARTESIAN_POINT('Origin',(8.,4.,7.));
#11434=CARTESIAN_POINT('Origin',(8.,4.,7.));
#11435=CARTESIAN_POINT('',(7.3,4.,7.));
#11436=CARTESIAN_POINT('Origin',(8.,4.,6.2));
#11437=CARTESIAN_POINT('',(7.7,4.,6.2));
#11438=CARTESIAN_POINT('',(7.7,4.,6.2));
#11439=CARTESIAN_POINT('Origin',(8.,4.,6.2));
#11440=CARTESIAN_POINT('Origin',(8.,4.,6.2));
#11441=CARTESIAN_POINT('',(7.7,4.,9.6));
#11442=CARTESIAN_POINT('Origin',(8.,4.,9.6));
#11443=CARTESIAN_POINT('',(7.7,4.,6.2));
#11444=CARTESIAN_POINT('Origin',(8.,4.,9.6));
#11445=CARTESIAN_POINT('Origin',(8.,4.,6.2));
#11446=CARTESIAN_POINT('',(0.,0.,0.));
#11447=CARTESIAN_POINT('Origin',(8.,4.,7.4));
#11448=CARTESIAN_POINT('',(7.695,4.,8.6));
#11449=CARTESIAN_POINT('Origin',(8.,4.,8.6));
#11450=CARTESIAN_POINT('',(7.695,4.,7.4));
#11451=CARTESIAN_POINT('',(7.695,4.,7.4));
#11452=CARTESIAN_POINT('Origin',(8.,4.,7.4));
#11453=CARTESIAN_POINT('Origin',(8.,4.,7.4));
#11454=CARTESIAN_POINT('',(7.5,4.,8.6));
#11455=CARTESIAN_POINT('Origin',(8.,4.,8.6));
#11456=CARTESIAN_POINT('',(7.5,4.,7.4));
#11457=CARTESIAN_POINT('',(7.5,4.,7.4));
#11458=CARTESIAN_POINT('Origin',(8.,4.,7.4));
#11459=CARTESIAN_POINT('Origin',(8.,4.,8.6));
#11460=CARTESIAN_POINT('Origin',(8.,4.,7.4));
#11461=CARTESIAN_POINT('',(0.,0.,0.));
#11462=CARTESIAN_POINT('Origin',(8.,4.,9.4));
#11463=CARTESIAN_POINT('',(7.695,4.,9.6));
#11464=CARTESIAN_POINT('Origin',(8.,4.,9.6));
#11465=CARTESIAN_POINT('',(7.695,4.,9.4));
#11466=CARTESIAN_POINT('',(7.695,4.,9.4));
#11467=CARTESIAN_POINT('Origin',(8.,4.,9.4));
#11468=CARTESIAN_POINT('Origin',(8.,4.,9.4));
#11469=CARTESIAN_POINT('',(7.5,4.,9.6));
#11470=CARTESIAN_POINT('Origin',(8.,4.,9.6));
#11471=CARTESIAN_POINT('',(7.5,4.,9.4));
#11472=CARTESIAN_POINT('',(7.5,4.,9.4));
#11473=CARTESIAN_POINT('Origin',(8.,4.,9.4));
#11474=CARTESIAN_POINT('Origin',(8.,4.,9.6));
#11475=CARTESIAN_POINT('Origin',(8.,4.,9.4));
#11476=CARTESIAN_POINT('',(0.,0.,0.));
#11477=CARTESIAN_POINT('Origin',(8.,4.,6.));
#11478=CARTESIAN_POINT('',(7.775,4.,6.2));
#11479=CARTESIAN_POINT('Origin',(8.,4.,6.2));
#11480=CARTESIAN_POINT('',(7.775,4.,6.));
#11481=CARTESIAN_POINT('',(7.775,4.,6.));
#11482=CARTESIAN_POINT('Origin',(8.,4.,6.));
#11483=CARTESIAN_POINT('Origin',(8.,4.,6.));
#11484=CARTESIAN_POINT('',(7.4,4.,6.2));
#11485=CARTESIAN_POINT('Origin',(8.,4.,6.2));
#11486=CARTESIAN_POINT('',(7.4,4.,6.));
#11487=CARTESIAN_POINT('',(7.4,4.,6.));
#11488=CARTESIAN_POINT('Origin',(8.,4.,6.));
#11489=CARTESIAN_POINT('Origin',(8.,4.,6.2));
#11490=CARTESIAN_POINT('Origin',(8.,4.,6.));
#11491=CARTESIAN_POINT('',(0.,0.,0.));
#11492=CARTESIAN_POINT('Origin',(8.,4.,9.6));
#11493=CARTESIAN_POINT('',(7.775,4.,9.8));
#11494=CARTESIAN_POINT('Origin',(8.,4.,9.8));
#11495=CARTESIAN_POINT('',(7.775,4.,9.6));
#11496=CARTESIAN_POINT('',(7.775,4.,9.6));
#11497=CARTESIAN_POINT('Origin',(8.,4.,9.6));
#11498=CARTESIAN_POINT('Origin',(8.,4.,9.6));
#11499=CARTESIAN_POINT('',(7.5,4.,9.8));
#11500=CARTESIAN_POINT('Origin',(8.,4.,9.8));
#11501=CARTESIAN_POINT('',(7.5,4.,9.6));
#11502=CARTESIAN_POINT('',(7.5,4.,9.6));
#11503=CARTESIAN_POINT('Origin',(8.,4.,9.6));
#11504=CARTESIAN_POINT('Origin',(8.,4.,9.8));
#11505=CARTESIAN_POINT('Origin',(8.,4.,9.6));
#11506=CARTESIAN_POINT('',(0.,0.,0.));
#11507=CARTESIAN_POINT('Origin',(0.,-0.4,0.));
#11508=CARTESIAN_POINT('',(-0.1954,-0.4,2.39295984553393E-17));
#11509=CARTESIAN_POINT('Origin',(0.,-0.4,0.));
#11510=CARTESIAN_POINT('Origin',(0.0577350269189626,0.,-0.1));
#11511=CARTESIAN_POINT('',(0.0577350269189626,0.,-0.1));
#11512=CARTESIAN_POINT('',(0.115470053837925,0.,0.));
#11513=CARTESIAN_POINT('',(0.0934187836487032,0.,-0.0381939203391614));
#11514=CARTESIAN_POINT('',(0.0577350269189626,-0.2,-0.1));
#11515=CARTESIAN_POINT('',(0.0577350269189626,0.,-0.1));
#11516=CARTESIAN_POINT('',(0.115470053837925,-0.2,0.));
#11517=CARTESIAN_POINT('',(0.115470053837925,-0.2,0.));
#11518=CARTESIAN_POINT('',(0.115470053837925,0.,0.));
#11519=CARTESIAN_POINT('Origin',(-0.0577350269189626,0.,-0.1));
#11520=CARTESIAN_POINT('',(-0.0577350269189626,0.,-0.1));
#11521=CARTESIAN_POINT('',(0.0561324865405187,0.,-0.1));
#11522=CARTESIAN_POINT('',(-0.0577350269189626,-0.2,-0.1));
#11523=CARTESIAN_POINT('',(-0.0577350269189626,0.,-0.1));
#11524=CARTESIAN_POINT('',(0.0577350269189626,-0.2,-0.1));
#11525=CARTESIAN_POINT('Origin',(-0.115470053837925,0.,-1.38777878078145E-17));
#11526=CARTESIAN_POINT('',(-0.115470053837925,0.,-1.41410031829988E-17));
#11527=CARTESIAN_POINT('',(-0.0797862971081845,0.,-0.0618060796608387));
#11528=CARTESIAN_POINT('',(-0.115470053837925,-0.2,-1.38777878078145E-17));
#11529=CARTESIAN_POINT('',(-0.115470053837925,0.,-1.41410031829988E-17));
#11530=CARTESIAN_POINT('',(-0.0577350269189626,-0.2,-0.1));
#11531=CARTESIAN_POINT('Origin',(-0.0577350269189626,0.,0.1));
#11532=CARTESIAN_POINT('',(-0.0577350269189626,0.,0.1));
#11533=CARTESIAN_POINT('',(-0.0509187836487033,0.,0.111806079660839));
#11534=CARTESIAN_POINT('',(-0.0577350269189626,-0.2,0.1));
#11535=CARTESIAN_POINT('',(-0.0577350269189626,0.,0.1));
#11536=CARTESIAN_POINT('',(-0.115470053837925,-0.2,-1.41410031829988E-17));
#11537=CARTESIAN_POINT('Origin',(0.0577350269189626,0.,0.1));
#11538=CARTESIAN_POINT('',(0.0577350269189626,0.,0.1));
#11539=CARTESIAN_POINT('',(0.113867513459481,0.,0.1));
#11540=CARTESIAN_POINT('',(0.0577350269189626,-0.2,0.1));
#11541=CARTESIAN_POINT('',(0.0577350269189626,0.,0.1));
#11542=CARTESIAN_POINT('',(-0.0577350269189626,-0.2,0.1));
#11543=CARTESIAN_POINT('Origin',(0.115470053837925,0.,0.));
#11544=CARTESIAN_POINT('',(0.122286297108185,0.,-0.0118060796608386));
#11545=CARTESIAN_POINT('',(0.0577350269189626,-0.2,0.1));
#11546=CARTESIAN_POINT('Origin',(0.,-0.2,0.));
#11547=CARTESIAN_POINT('Origin',(0.17,0.,0.));
#11548=CARTESIAN_POINT('',(-0.17,-8.67361737988404E-18,-2.0818995585505E-17));
#11549=CARTESIAN_POINT('Origin',(0.,0.,0.));
#11550=CARTESIAN_POINT('Origin',(0.,-0.015,0.));
#11551=CARTESIAN_POINT('',(-0.1954,-0.0254,-2.39295984553393E-17));
#11552=CARTESIAN_POINT('Origin',(0.,-0.0254,0.));
#11553=CARTESIAN_POINT('',(-0.185,-0.015,-2.2655965784226E-17));
#11554=CARTESIAN_POINT('Origin',(0.,-0.2775,0.));
#11555=CARTESIAN_POINT('',(-0.1954,-0.2775,-2.39295984553393E-17));
#11556=CARTESIAN_POINT('',(0.,0.,0.));
#11557=CARTESIAN_POINT('Origin',(0.3,0.4,0.));
#11558=CARTESIAN_POINT('',(-0.3,0.4,-3.67394039744206E-17));
#11559=CARTESIAN_POINT('Origin',(0.,0.4,0.));
#11560=CARTESIAN_POINT('Origin',(0.,0.375,0.));
#11561=CARTESIAN_POINT('',(-0.35,0.35,-4.28626379701573E-17));
#11562=CARTESIAN_POINT('Origin',(0.,0.35,0.));
#11563=CARTESIAN_POINT('',(-0.325,0.375,-3.9801020972289E-17));
#11564=CARTESIAN_POINT('Origin',(0.,0.19,0.));
#11565=CARTESIAN_POINT('',(-0.35,0.03,-4.28626379701574E-17));
#11566=CARTESIAN_POINT('Origin',(0.,0.03,0.));
#11567=CARTESIAN_POINT('',(-0.35,0.19,-4.28626379701574E-17));
#11568=CARTESIAN_POINT('Origin',(0.,0.0149999999999999,0.));
#11569=CARTESIAN_POINT('',(-0.32,-3.29597460435593E-17,-3.91886975727153E-17));
#11570=CARTESIAN_POINT('Origin',(0.,0.,0.));
#11571=CARTESIAN_POINT('',(-0.335,0.0149999999999999,-4.10256677714363E-17));
#11572=CARTESIAN_POINT('Origin',(0.22,0.,0.));
#11573=CARTESIAN_POINT('',(-0.22,-6.93889390390723E-18,-2.69422295812418E-17));
#11574=CARTESIAN_POINT('Origin',(0.,0.,0.));
#11575=CARTESIAN_POINT('Origin',(0.,-0.02,0.));
#11576=CARTESIAN_POINT('',(-0.1954,-0.0492,2.39295984553393E-17));
#11577=CARTESIAN_POINT('Origin',(0.,-0.0492,0.));
#11578=CARTESIAN_POINT('',(-0.21,-0.02,-2.57175827820944E-17));
#11579=CARTESIAN_POINT('Origin',(0.,-0.8,0.));
#11580=CARTESIAN_POINT('',(-0.1954,-1.5646,2.39295984553393E-17));
#11581=CARTESIAN_POINT('Origin',(0.,-1.5646,0.));
#11582=CARTESIAN_POINT('',(-0.1954,-0.8,-2.39295984553393E-17));
#11583=CARTESIAN_POINT('Origin',(0.,-1.58,0.));
#11584=CARTESIAN_POINT('',(-0.16,-1.6,-1.95943487863577E-17));
#11585=CARTESIAN_POINT('Origin',(0.,-1.6,0.));
#11586=CARTESIAN_POINT('',(-0.18,-1.58,-2.20436423846524E-17));
#11587=CARTESIAN_POINT('Origin',(0.,-1.6,0.));
#11588=CARTESIAN_POINT('Origin',(0.0866025403784439,-0.4,-0.15));
#11589=CARTESIAN_POINT('',(0.173205080756888,-0.4,0.));
#11590=CARTESIAN_POINT('',(0.0866025403784439,-0.4,-0.15));
#11591=CARTESIAN_POINT('',(0.173205080756888,-0.4,0.));
#11592=CARTESIAN_POINT('',(0.0866025403784439,-0.64,-0.15));
#11593=CARTESIAN_POINT('',(0.0866025403784439,-0.4,-0.15));
#11594=CARTESIAN_POINT('',(0.173205080756888,-0.64,0.));
#11595=CARTESIAN_POINT('',(0.173205080756888,-0.64,0.));
#11596=CARTESIAN_POINT('',(0.173205080756888,-0.4,0.));
#11597=CARTESIAN_POINT('Origin',(-0.0866025403784438,-0.4,-0.15));
#11598=CARTESIAN_POINT('',(-0.0866025403784438,-0.4,-0.15));
#11599=CARTESIAN_POINT('',(0.0866025403784439,-0.4,-0.15));
#11600=CARTESIAN_POINT('',(-0.0866025403784438,-0.64,-0.15));
#11601=CARTESIAN_POINT('',(-0.0866025403784438,-0.4,-0.15));
#11602=CARTESIAN_POINT('',(0.0866025403784439,-0.64,-0.15));
#11603=CARTESIAN_POINT('Origin',(-0.173205080756888,-0.4,-2.77555756156289E-17));
#11604=CARTESIAN_POINT('',(-0.173205080756888,-0.4,-2.12115047744981E-17));
#11605=CARTESIAN_POINT('',(-0.0866025403784438,-0.4,-0.15));
#11606=CARTESIAN_POINT('',(-0.173205080756888,-0.64,-2.77555756156289E-17));
#11607=CARTESIAN_POINT('',(-0.173205080756888,-0.4,-2.12115047744981E-17));
#11608=CARTESIAN_POINT('',(-0.0866025403784438,-0.64,-0.15));
#11609=CARTESIAN_POINT('Origin',(-0.0866025403784439,-0.4,0.15));
#11610=CARTESIAN_POINT('',(-0.0866025403784439,-0.4,0.15));
#11611=CARTESIAN_POINT('',(-0.173205080756888,-0.4,-2.12115047744981E-17));
#11612=CARTESIAN_POINT('',(-0.0866025403784439,-0.64,0.15));
#11613=CARTESIAN_POINT('',(-0.0866025403784439,-0.4,0.15));
#11614=CARTESIAN_POINT('',(-0.173205080756888,-0.64,-2.12115047744981E-17));
#11615=CARTESIAN_POINT('Origin',(0.0866025403784439,-0.4,0.15));
#11616=CARTESIAN_POINT('',(0.0866025403784439,-0.4,0.15));
#11617=CARTESIAN_POINT('',(-0.0866025403784439,-0.4,0.15));
#11618=CARTESIAN_POINT('',(0.0866025403784439,-0.64,0.15));
#11619=CARTESIAN_POINT('',(0.0866025403784439,-0.4,0.15));
#11620=CARTESIAN_POINT('',(-0.0866025403784439,-0.64,0.15));
#11621=CARTESIAN_POINT('Origin',(0.173205080756888,-0.4,0.));
#11622=CARTESIAN_POINT('',(0.0866025403784439,-0.4,0.15));
#11623=CARTESIAN_POINT('',(0.0866025403784439,-0.64,0.15));
#11624=CARTESIAN_POINT('Origin',(0.,-0.4,-2.77555756156289E-17));
#11625=CARTESIAN_POINT('Origin',(0.,-0.64,-2.77555756156289E-17));
#11626=CARTESIAN_POINT('',(0.,0.,0.));
#11627=CARTESIAN_POINT('Origin',(0.0866025403784439,-0.4,-0.15));
#11628=CARTESIAN_POINT('',(0.173205080756888,-0.4,0.));
#11629=CARTESIAN_POINT('',(0.0866025403784439,-0.4,-0.15));
#11630=CARTESIAN_POINT('',(0.173205080756888,-0.4,0.));
#11631=CARTESIAN_POINT('',(0.0866025403784439,-0.64,-0.15));
#11632=CARTESIAN_POINT('',(0.0866025403784439,-0.4,-0.15));
#11633=CARTESIAN_POINT('',(0.173205080756888,-0.64,0.));
#11634=CARTESIAN_POINT('',(0.173205080756888,-0.64,0.));
#11635=CARTESIAN_POINT('',(0.173205080756888,-0.4,0.));
#11636=CARTESIAN_POINT('Origin',(-0.0866025403784438,-0.4,-0.15));
#11637=CARTESIAN_POINT('',(-0.0866025403784438,-0.4,-0.15));
#11638=CARTESIAN_POINT('',(0.0866025403784439,-0.4,-0.15));
#11639=CARTESIAN_POINT('',(-0.0866025403784438,-0.64,-0.15));
#11640=CARTESIAN_POINT('',(-0.0866025403784438,-0.4,-0.15));
#11641=CARTESIAN_POINT('',(0.0866025403784439,-0.64,-0.15));
#11642=CARTESIAN_POINT('Origin',(-0.173205080756888,-0.4,-2.77555756156289E-17));
#11643=CARTESIAN_POINT('',(-0.173205080756888,-0.4,-2.12115047744981E-17));
#11644=CARTESIAN_POINT('',(-0.0866025403784438,-0.4,-0.15));
#11645=CARTESIAN_POINT('',(-0.173205080756888,-0.64,-2.77555756156289E-17));
#11646=CARTESIAN_POINT('',(-0.173205080756888,-0.4,-2.12115047744981E-17));
#11647=CARTESIAN_POINT('',(-0.0866025403784438,-0.64,-0.15));
#11648=CARTESIAN_POINT('Origin',(-0.0866025403784439,-0.4,0.15));
#11649=CARTESIAN_POINT('',(-0.0866025403784439,-0.4,0.15));
#11650=CARTESIAN_POINT('',(-0.173205080756888,-0.4,-2.12115047744981E-17));
#11651=CARTESIAN_POINT('',(-0.0866025403784439,-0.64,0.15));
#11652=CARTESIAN_POINT('',(-0.0866025403784439,-0.4,0.15));
#11653=CARTESIAN_POINT('',(-0.173205080756888,-0.64,-2.12115047744981E-17));
#11654=CARTESIAN_POINT('Origin',(0.0866025403784439,-0.4,0.15));
#11655=CARTESIAN_POINT('',(0.0866025403784439,-0.4,0.15));
#11656=CARTESIAN_POINT('',(-0.0866025403784439,-0.4,0.15));
#11657=CARTESIAN_POINT('',(0.0866025403784439,-0.64,0.15));
#11658=CARTESIAN_POINT('',(0.0866025403784439,-0.4,0.15));
#11659=CARTESIAN_POINT('',(-0.0866025403784439,-0.64,0.15));
#11660=CARTESIAN_POINT('Origin',(0.173205080756888,-0.4,0.));
#11661=CARTESIAN_POINT('',(0.0866025403784439,-0.4,0.15));
#11662=CARTESIAN_POINT('',(0.0866025403784439,-0.64,0.15));
#11663=CARTESIAN_POINT('Origin',(0.,-0.4,-2.77555756156289E-17));
#11664=CARTESIAN_POINT('Origin',(0.,-0.64,-2.77555756156289E-17));
#11665=CARTESIAN_POINT('Origin',(0.,-1.,0.));
#11666=CARTESIAN_POINT('',(-0.1954,-1.,2.39295984553393E-17));
#11667=CARTESIAN_POINT('Origin',(0.,-1.,0.));
#11668=CARTESIAN_POINT('Origin',(0.3,0.4,0.));
#11669=CARTESIAN_POINT('',(-0.3,0.4,-3.67394039744206E-17));
#11670=CARTESIAN_POINT('Origin',(0.,0.4,0.));
#11671=CARTESIAN_POINT('Origin',(0.,0.375,0.));
#11672=CARTESIAN_POINT('',(-0.35,0.35,-4.28626379701573E-17));
#11673=CARTESIAN_POINT('Origin',(0.,0.35,0.));
#11674=CARTESIAN_POINT('',(-0.325,0.375,-3.9801020972289E-17));
#11675=CARTESIAN_POINT('Origin',(0.,0.19,0.));
#11676=CARTESIAN_POINT('',(-0.35,0.03,-4.28626379701574E-17));
#11677=CARTESIAN_POINT('Origin',(0.,0.03,0.));
#11678=CARTESIAN_POINT('',(-0.35,0.19,-4.28626379701574E-17));
#11679=CARTESIAN_POINT('Origin',(0.,0.0149999999999999,0.));
#11680=CARTESIAN_POINT('',(-0.32,-3.29597460435593E-17,-3.91886975727153E-17));
#11681=CARTESIAN_POINT('Origin',(0.,0.,0.));
#11682=CARTESIAN_POINT('',(-0.335,0.0149999999999999,-4.10256677714363E-17));
#11683=CARTESIAN_POINT('Origin',(0.22,0.,0.));
#11684=CARTESIAN_POINT('',(-0.22,-6.93889390390723E-18,-2.69422295812418E-17));
#11685=CARTESIAN_POINT('Origin',(0.,0.,0.));
#11686=CARTESIAN_POINT('Origin',(0.,-0.02,0.));
#11687=CARTESIAN_POINT('',(-0.1954,-0.0492,2.39295984553393E-17));
#11688=CARTESIAN_POINT('Origin',(0.,-0.0492,0.));
#11689=CARTESIAN_POINT('',(-0.21,-0.02,-2.57175827820944E-17));
#11690=CARTESIAN_POINT('Origin',(0.,-0.8,0.));
#11691=CARTESIAN_POINT('',(-0.1954,-0.8,-2.39295984553393E-17));
#11692=CARTESIAN_POINT('',(0.,0.,0.));
#11693=CARTESIAN_POINT('',(0.,0.,0.));
#11694=CARTESIAN_POINT('',(0.,0.,0.));
#11695=CARTESIAN_POINT('',(0.,0.,0.));
#11696=CARTESIAN_POINT('',(0.,0.,0.));
#11697=CARTESIAN_POINT('',(0.,0.,0.));
#11698=CARTESIAN_POINT('',(0.,0.,0.));
#11699=CARTESIAN_POINT('',(0.,0.,0.));
#11700=CARTESIAN_POINT('',(1.76776695296637,1.76776695296637,1.8));
#11701=CARTESIAN_POINT('',(-1.76776695296637,1.76776695296637,1.8));
#11702=CARTESIAN_POINT('',(-1.76776695296637,-1.76776695296637,1.8));
#11703=CARTESIAN_POINT('',(1.76776695296637,-1.76776695296637,1.8));
#11704=CARTESIAN_POINT('',(0.,0.,2.5));
#11705=CARTESIAN_POINT('',(0.,0.,4.5));
#11706=CARTESIAN_POINT('',(1.23743686707646,1.23743686707646,5.6));
#11707=CARTESIAN_POINT('',(-1.23743686707646,1.23743686707646,5.6));
#11708=CARTESIAN_POINT('',(-1.23743686707646,-1.23743686707646,5.6));
#11709=CARTESIAN_POINT('',(1.23743686707646,-1.23743686707646,5.6));
#11710=CARTESIAN_POINT('',(9.76776695296637,1.76776695296637,1.8));
#11711=CARTESIAN_POINT('',(6.23223304703363,1.76776695296637,1.8));
#11712=CARTESIAN_POINT('',(6.23223304703363,-1.76776695296637,1.8));
#11713=CARTESIAN_POINT('',(9.76776695296637,-1.76776695296637,1.8));
#11714=CARTESIAN_POINT('',(8.,0.,3.5));
#11715=CARTESIAN_POINT('',(9.23743686707646,1.23743686707646,5.6));
#11716=CARTESIAN_POINT('',(6.76256313292354,1.23743686707646,5.6));
#11717=CARTESIAN_POINT('',(6.76256313292354,-1.23743686707646,5.6));
#11718=CARTESIAN_POINT('',(9.23743686707646,-1.23743686707646,5.6));
#11719=CARTESIAN_POINT('',(0.,0.,0.));
#11720=CARTESIAN_POINT('',(0.,0.,0.));
#11721=CARTESIAN_POINT('',(0.,0.,0.));
#11722=CARTESIAN_POINT('',(0.,0.,0.));
#11723=CARTESIAN_POINT('',(0.,0.,0.));
#11724=CARTESIAN_POINT('',(0.,0.,0.));
#11725=CARTESIAN_POINT('',(0.,0.,0.));
#11726=CARTESIAN_POINT('',(0.,0.,0.));
#11727=CARTESIAN_POINT('',(0.,0.,0.));
#11728=CARTESIAN_POINT('',(0.,0.,0.));
#11729=CARTESIAN_POINT('',(0.,0.,0.));
#11730=CARTESIAN_POINT('',(0.9,0.,1.4));
#11731=CARTESIAN_POINT('',(1.1,0.,7.5));
#11732=CARTESIAN_POINT('',(0.,2.22044604925031E-16,8.2));
#11733=CARTESIAN_POINT('',(-0.429855350392604,2.61349944954989,6.));
#11734=CARTESIAN_POINT('',(-0.429855350392604,2.61349944954989,9.8));
#11735=CARTESIAN_POINT('',(0.,0.,0.));
#11736=CARTESIAN_POINT('',(0.,0.,0.));
#11737=CARTESIAN_POINT('',(0.,0.,0.));
#11738=CARTESIAN_POINT('',(0.,0.,0.));
#11739=CARTESIAN_POINT('',(0.,0.,0.));
#11740=CARTESIAN_POINT('',(0.,0.,0.));
#11741=CARTESIAN_POINT('',(0.,0.,0.));
#11742=CARTESIAN_POINT('',(0.,0.,0.));
#11743=CARTESIAN_POINT('',(8.9,0.,1.4));
#11744=CARTESIAN_POINT('',(8.,4.,6.));
#11745=CARTESIAN_POINT('',(8.,4.,9.8));
#11746=CARTESIAN_POINT('',(0.,0.,0.));
#11747=CARTESIAN_POINT('',(0.,0.,0.));
#11748=CARTESIAN_POINT('Origin',(-0.429855350392604,2.61349944954989,8.5));
#11749=CARTESIAN_POINT('',(-0.929855350392604,2.61349944954989,8.6));
#11750=CARTESIAN_POINT('Origin',(-0.429855350392604,2.61349944954989,8.6));
#11751=CARTESIAN_POINT('',(-0.929855350392604,2.61349944954989,9.4));
#11752=CARTESIAN_POINT('',(-0.929855350392604,2.61349944954989,8.5));
#11753=CARTESIAN_POINT('Origin',(-0.429855350392604,2.61349944954989,9.4));
#11754=CARTESIAN_POINT('Origin',(8.,4.,8.5));
#11755=CARTESIAN_POINT('',(7.5,4.,8.6));
#11756=CARTESIAN_POINT('Origin',(8.,4.,8.6));
#11757=CARTESIAN_POINT('',(7.5,4.,9.4));
#11758=CARTESIAN_POINT('',(7.5,4.,8.5));
#11759=CARTESIAN_POINT('Origin',(8.,4.,9.4));
#11760=CARTESIAN_POINT('Origin',(8.,4.,8.6));
#11761=CARTESIAN_POINT('',(7.06430880824222,4.35282005848151,9.4));
#11762=CARTESIAN_POINT('',(7.06430880824222,4.35282005848151,8.6));
#11763=CARTESIAN_POINT('',(7.06430880824222,4.35282005848151,8.6));
#11764=CARTESIAN_POINT('',(7.22660327051141,3.36607768708118,9.4));
#11765=CARTESIAN_POINT('Origin',(8.,4.,9.4));
#11766=CARTESIAN_POINT('',(7.22660327051141,3.36607768708118,8.6));
#11767=CARTESIAN_POINT('',(7.22660327051141,3.36607768708118,8.6));
#11768=CARTESIAN_POINT('Origin',(8.,4.,8.6));
#11769=CARTESIAN_POINT('Origin',(7.91885276886541,4.49337118570017,8.6));
#11770=CARTESIAN_POINT('',(0.34354137909599,3.24742176246871,8.6));
#11771=CARTESIAN_POINT('',(-0.511002581527199,3.10687063525006,8.6));
#11772=CARTESIAN_POINT('',(0.34354137909599,3.24742176246871,9.4));
#11773=CARTESIAN_POINT('',(0.343541379095991,3.24742176246871,8.6));
#11774=CARTESIAN_POINT('',(-0.511002581527199,3.10687063525006,9.4));
#11775=CARTESIAN_POINT('Origin',(-0.429855350392604,2.61349944954989,8.6));
#11776=CARTESIAN_POINT('',(0.505835841365177,2.26067939106837,8.6));
#11777=CARTESIAN_POINT('',(8.08114723113459,3.50662881429983,8.6));
#11778=CARTESIAN_POINT('Origin',(-0.429855350392604,2.61349944954989,8.6));
#11779=CARTESIAN_POINT('Origin',(-0.34870811925801,2.12012826384972,8.6));
#11780=CARTESIAN_POINT('',(0.505835841365177,2.26067939106837,9.4));
#11781=CARTESIAN_POINT('',(8.08114723113459,3.50662881429983,9.4));
#11782=CARTESIAN_POINT('',(0.505835841365179,2.26067939106837,8.6));
#11783=CARTESIAN_POINT('Origin',(-0.429855350392604,2.61349944954989,8.6));
#11784=CARTESIAN_POINT('Origin',(-0.429855350392604,2.61349944954989,9.4));
#11785=CARTESIAN_POINT('Origin',(-0.429855350392604,2.61349944954989,9.4));
#11786=CARTESIAN_POINT('',(0.,0.,0.));
#11787=CARTESIAN_POINT('Origin',(-0.429855350392604,2.61349944954989,8.6));
#11788=CARTESIAN_POINT('',(-0.734855350392604,2.61349944954989,9.4));
#11789=CARTESIAN_POINT('Origin',(-0.429855350392604,2.61349944954989,9.4));
#11790=CARTESIAN_POINT('',(-0.734855350392604,2.61349944954989,8.6));
#11791=CARTESIAN_POINT('',(-0.734855350392604,2.61349944954989,8.6));
#11792=CARTESIAN_POINT('Origin',(-0.429855350392604,2.61349944954989,8.6));
#11793=CARTESIAN_POINT('Origin',(-0.429855350392604,2.61349944954989,8.6));
#11794=CARTESIAN_POINT('',(-0.929855350392604,2.61349944954989,9.4));
#11795=CARTESIAN_POINT('Origin',(-0.429855350392604,2.61349944954989,9.4));
#11796=CARTESIAN_POINT('',(-0.929855350392604,2.61349944954989,8.6));
#11797=CARTESIAN_POINT('',(-0.929855350392604,2.61349944954989,8.6));
#11798=CARTESIAN_POINT('Origin',(-0.429855350392604,2.61349944954989,8.6));
#11799=CARTESIAN_POINT('Origin',(-0.429855350392604,2.61349944954989,9.4));
#11800=CARTESIAN_POINT('Origin',(-0.429855350392604,2.61349944954989,8.6));
#11801=CARTESIAN_POINT('',(0.,0.,0.));
#11802=CARTESIAN_POINT('Origin',(8.,4.,8.6));
#11803=CARTESIAN_POINT('',(7.695,4.,9.4));
#11804=CARTESIAN_POINT('Origin',(8.,4.,9.4));
#11805=CARTESIAN_POINT('',(7.695,4.,8.6));
#11806=CARTESIAN_POINT('',(7.695,4.,8.6));
#11807=CARTESIAN_POINT('Origin',(8.,4.,8.6));
#11808=CARTESIAN_POINT('Origin',(8.,4.,8.6));
#11809=CARTESIAN_POINT('',(7.5,4.,9.4));
#11810=CARTESIAN_POINT('Origin',(8.,4.,9.4));
#11811=CARTESIAN_POINT('',(7.5,4.,8.6));
#11812=CARTESIAN_POINT('',(7.5,4.,8.6));
#11813=CARTESIAN_POINT('Origin',(8.,4.,8.6));
#11814=CARTESIAN_POINT('Origin',(8.,4.,9.4));
#11815=CARTESIAN_POINT('Origin',(8.,4.,8.6));
#11816=CARTESIAN_POINT('',(0.,0.,0.));
#11817=CARTESIAN_POINT('',(0.,0.,0.));
#11818=CARTESIAN_POINT('',(0.,0.,0.));
#11819=CARTESIAN_POINT('',(0.,0.,0.));
#11820=CARTESIAN_POINT('',(0.,0.,0.));
#11821=CARTESIAN_POINT('',(0.,0.,0.));
#11822=CARTESIAN_POINT('',(0.,0.,0.));
#11823=UNCERTAINTY_MEASURE_WITH_UNIT(LENGTH_MEASURE(0.001),#11917,
'DISTANCE_ACCURACY_VALUE',
'Maximum model space distance between geometric entities at asserted c
onnectivities');
#11824=UNCERTAINTY_MEASURE_WITH_UNIT(LENGTH_MEASURE(0.001),#11917,
'DISTANCE_ACCURACY_VALUE',
'Maximum model space distance between geometric entities at asserted c
onnectivities');
#11825=UNCERTAINTY_MEASURE_WITH_UNIT(LENGTH_MEASURE(0.001),#11917,
'DISTANCE_ACCURACY_VALUE',
'Maximum model space distance between geometric entities at asserted c
onnectivities');
#11826=UNCERTAINTY_MEASURE_WITH_UNIT(LENGTH_MEASURE(0.001),#11917,
'DISTANCE_ACCURACY_VALUE',
'Maximum model space distance between geometric entities at asserted c
onnectivities');
#11827=UNCERTAINTY_MEASURE_WITH_UNIT(LENGTH_MEASURE(0.001),#11917,
'DISTANCE_ACCURACY_VALUE',
'Maximum model space distance between geometric entities at asserted c
onnectivities');
#11828=UNCERTAINTY_MEASURE_WITH_UNIT(LENGTH_MEASURE(0.001),#11917,
'DISTANCE_ACCURACY_VALUE',
'Maximum model space distance between geometric entities at asserted c
onnectivities');
#11829=UNCERTAINTY_MEASURE_WITH_UNIT(LENGTH_MEASURE(0.001),#11917,
'DISTANCE_ACCURACY_VALUE',
'Maximum model space distance between geometric entities at asserted c
onnectivities');
#11830=UNCERTAINTY_MEASURE_WITH_UNIT(LENGTH_MEASURE(0.001),#11917,
'DISTANCE_ACCURACY_VALUE',
'Maximum model space distance between geometric entities at asserted c
onnectivities');
#11831=UNCERTAINTY_MEASURE_WITH_UNIT(LENGTH_MEASURE(0.001),#11917,
'DISTANCE_ACCURACY_VALUE',
'Maximum model space distance between geometric entities at asserted c
onnectivities');
#11832=UNCERTAINTY_MEASURE_WITH_UNIT(LENGTH_MEASURE(0.001),#11917,
'DISTANCE_ACCURACY_VALUE',
'Maximum model space distance between geometric entities at asserted c
onnectivities');
#11833=UNCERTAINTY_MEASURE_WITH_UNIT(LENGTH_MEASURE(0.001),#11917,
'DISTANCE_ACCURACY_VALUE',
'Maximum model space distance between geometric entities at asserted c
onnectivities');
#11834=UNCERTAINTY_MEASURE_WITH_UNIT(LENGTH_MEASURE(0.001),#11917,
'DISTANCE_ACCURACY_VALUE',
'Maximum model space distance between geometric entities at asserted c
onnectivities');
#11835=UNCERTAINTY_MEASURE_WITH_UNIT(LENGTH_MEASURE(0.001),#11917,
'DISTANCE_ACCURACY_VALUE',
'Maximum model space distance between geometric entities at asserted c
onnectivities');
#11836=UNCERTAINTY_MEASURE_WITH_UNIT(LENGTH_MEASURE(0.001),#11917,
'DISTANCE_ACCURACY_VALUE',
'Maximum model space distance between geometric entities at asserted c
onnectivities');
#11837=UNCERTAINTY_MEASURE_WITH_UNIT(LENGTH_MEASURE(0.001),#11917,
'DISTANCE_ACCURACY_VALUE',
'Maximum model space distance between geometric entities at asserted c
onnectivities');
#11838=UNCERTAINTY_MEASURE_WITH_UNIT(LENGTH_MEASURE(0.001),#11917,
'DISTANCE_ACCURACY_VALUE',
'Maximum model space distance between geometric entities at asserted c
onnectivities');
#11839=UNCERTAINTY_MEASURE_WITH_UNIT(LENGTH_MEASURE(0.001),#11917,
'DISTANCE_ACCURACY_VALUE',
'Maximum model space distance between geometric entities at asserted c
onnectivities');
#11840=UNCERTAINTY_MEASURE_WITH_UNIT(LENGTH_MEASURE(0.001),#11917,
'DISTANCE_ACCURACY_VALUE',
'Maximum model space distance between geometric entities at asserted c
onnectivities');
#11841=UNCERTAINTY_MEASURE_WITH_UNIT(LENGTH_MEASURE(0.001),#11917,
'DISTANCE_ACCURACY_VALUE',
'Maximum model space distance between geometric entities at asserted c
onnectivities');
#11842=UNCERTAINTY_MEASURE_WITH_UNIT(LENGTH_MEASURE(0.001),#11917,
'DISTANCE_ACCURACY_VALUE',
'Maximum model space distance between geometric entities at asserted c
onnectivities');
#11843=UNCERTAINTY_MEASURE_WITH_UNIT(LENGTH_MEASURE(0.001),#11917,
'DISTANCE_ACCURACY_VALUE',
'Maximum model space distance between geometric entities at asserted c
onnectivities');
#11844=UNCERTAINTY_MEASURE_WITH_UNIT(LENGTH_MEASURE(0.001),#11917,
'DISTANCE_ACCURACY_VALUE',
'Maximum model space distance between geometric entities at asserted c
onnectivities');
#11845=UNCERTAINTY_MEASURE_WITH_UNIT(LENGTH_MEASURE(0.001),#11917,
'DISTANCE_ACCURACY_VALUE',
'Maximum model space distance between geometric entities at asserted c
onnectivities');
#11846=UNCERTAINTY_MEASURE_WITH_UNIT(LENGTH_MEASURE(0.001),#11917,
'DISTANCE_ACCURACY_VALUE',
'Maximum model space distance between geometric entities at asserted c
onnectivities');
#11847=UNCERTAINTY_MEASURE_WITH_UNIT(LENGTH_MEASURE(0.001),#11917,
'DISTANCE_ACCURACY_VALUE',
'Maximum model space distance between geometric entities at asserted c
onnectivities');
#11848=UNCERTAINTY_MEASURE_WITH_UNIT(LENGTH_MEASURE(0.001),#11917,
'DISTANCE_ACCURACY_VALUE',
'Maximum model space distance between geometric entities at asserted c
onnectivities');
#11849=UNCERTAINTY_MEASURE_WITH_UNIT(LENGTH_MEASURE(0.001),#11917,
'DISTANCE_ACCURACY_VALUE',
'Maximum model space distance between geometric entities at asserted c
onnectivities');
#11850=UNCERTAINTY_MEASURE_WITH_UNIT(LENGTH_MEASURE(0.001),#11917,
'DISTANCE_ACCURACY_VALUE',
'Maximum model space distance between geometric entities at asserted c
onnectivities');
#11851=UNCERTAINTY_MEASURE_WITH_UNIT(LENGTH_MEASURE(0.001),#11917,
'DISTANCE_ACCURACY_VALUE',
'Maximum model space distance between geometric entities at asserted c
onnectivities');
#11852=UNCERTAINTY_MEASURE_WITH_UNIT(LENGTH_MEASURE(0.001),#11917,
'DISTANCE_ACCURACY_VALUE',
'Maximum model space distance between geometric entities at asserted c
onnectivities');
#11853=UNCERTAINTY_MEASURE_WITH_UNIT(LENGTH_MEASURE(0.001),#11917,
'DISTANCE_ACCURACY_VALUE',
'Maximum model space distance between geometric entities at asserted c
onnectivities');
#11854=UNCERTAINTY_MEASURE_WITH_UNIT(LENGTH_MEASURE(0.001),#11917,
'DISTANCE_ACCURACY_VALUE',
'Maximum model space distance between geometric entities at asserted c
onnectivities');
#11855=UNCERTAINTY_MEASURE_WITH_UNIT(LENGTH_MEASURE(0.001),#11917,
'DISTANCE_ACCURACY_VALUE',
'Maximum model space distance between geometric entities at asserted c
onnectivities');
#11856=UNCERTAINTY_MEASURE_WITH_UNIT(LENGTH_MEASURE(0.001),#11917,
'DISTANCE_ACCURACY_VALUE',
'Maximum model space distance between geometric entities at asserted c
onnectivities');
#11857=UNCERTAINTY_MEASURE_WITH_UNIT(LENGTH_MEASURE(0.001),#11917,
'DISTANCE_ACCURACY_VALUE',
'Maximum model space distance between geometric entities at asserted c
onnectivities');
#11858=UNCERTAINTY_MEASURE_WITH_UNIT(LENGTH_MEASURE(0.001),#11917,
'DISTANCE_ACCURACY_VALUE',
'Maximum model space distance between geometric entities at asserted c
onnectivities');
#11859=UNCERTAINTY_MEASURE_WITH_UNIT(LENGTH_MEASURE(0.001),#11917,
'DISTANCE_ACCURACY_VALUE',
'Maximum model space distance between geometric entities at asserted c
onnectivities');
#11860=UNCERTAINTY_MEASURE_WITH_UNIT(LENGTH_MEASURE(0.001),#11917,
'DISTANCE_ACCURACY_VALUE',
'Maximum model space distance between geometric entities at asserted c
onnectivities');
#11861=UNCERTAINTY_MEASURE_WITH_UNIT(LENGTH_MEASURE(0.001),#11917,
'DISTANCE_ACCURACY_VALUE',
'Maximum model space distance between geometric entities at asserted c
onnectivities');
#11862=UNCERTAINTY_MEASURE_WITH_UNIT(LENGTH_MEASURE(0.001),#11917,
'DISTANCE_ACCURACY_VALUE',
'Maximum model space distance between geometric entities at asserted c
onnectivities');
#11863=UNCERTAINTY_MEASURE_WITH_UNIT(LENGTH_MEASURE(0.001),#11917,
'DISTANCE_ACCURACY_VALUE',
'Maximum model space distance between geometric entities at asserted c
onnectivities');
#11864=UNCERTAINTY_MEASURE_WITH_UNIT(LENGTH_MEASURE(0.001),#11917,
'DISTANCE_ACCURACY_VALUE',
'Maximum model space distance between geometric entities at asserted c
onnectivities');
#11865=UNCERTAINTY_MEASURE_WITH_UNIT(LENGTH_MEASURE(0.001),#11917,
'DISTANCE_ACCURACY_VALUE',
'Maximum model space distance between geometric entities at asserted c
onnectivities');
#11866=UNCERTAINTY_MEASURE_WITH_UNIT(LENGTH_MEASURE(0.001),#11917,
'DISTANCE_ACCURACY_VALUE',
'Maximum model space distance between geometric entities at asserted c
onnectivities');
#11867=UNCERTAINTY_MEASURE_WITH_UNIT(LENGTH_MEASURE(0.001),#11917,
'DISTANCE_ACCURACY_VALUE',
'Maximum model space distance between geometric entities at asserted c
onnectivities');
#11868=UNCERTAINTY_MEASURE_WITH_UNIT(LENGTH_MEASURE(0.001),#11917,
'DISTANCE_ACCURACY_VALUE',
'Maximum model space distance between geometric entities at asserted c
onnectivities');
#11869=UNCERTAINTY_MEASURE_WITH_UNIT(LENGTH_MEASURE(0.001),#11917,
'DISTANCE_ACCURACY_VALUE',
'Maximum model space distance between geometric entities at asserted c
onnectivities');
#11870=(
GEOMETRIC_REPRESENTATION_CONTEXT(3)
GLOBAL_UNCERTAINTY_ASSIGNED_CONTEXT((#11823))
GLOBAL_UNIT_ASSIGNED_CONTEXT((#11917,#11919,#11920))
REPRESENTATION_CONTEXT('','3D')
);
#11871=(
GEOMETRIC_REPRESENTATION_CONTEXT(3)
GLOBAL_UNCERTAINTY_ASSIGNED_CONTEXT((#11824))
GLOBAL_UNIT_ASSIGNED_CONTEXT((#11917,#11919,#11920))
REPRESENTATION_CONTEXT('','3D')
);
#11872=(
GEOMETRIC_REPRESENTATION_CONTEXT(3)
GLOBAL_UNCERTAINTY_ASSIGNED_CONTEXT((#11825))
GLOBAL_UNIT_ASSIGNED_CONTEXT((#11917,#11919,#11920))
REPRESENTATION_CONTEXT('','3D')
);
#11873=(
GEOMETRIC_REPRESENTATION_CONTEXT(3)
GLOBAL_UNCERTAINTY_ASSIGNED_CONTEXT((#11826))
GLOBAL_UNIT_ASSIGNED_CONTEXT((#11917,#11919,#11920))
REPRESENTATION_CONTEXT('','3D')
);
#11874=(
GEOMETRIC_REPRESENTATION_CONTEXT(3)
GLOBAL_UNCERTAINTY_ASSIGNED_CONTEXT((#11827))
GLOBAL_UNIT_ASSIGNED_CONTEXT((#11917,#11919,#11920))
REPRESENTATION_CONTEXT('','3D')
);
#11875=(
GEOMETRIC_REPRESENTATION_CONTEXT(3)
GLOBAL_UNCERTAINTY_ASSIGNED_CONTEXT((#11828))
GLOBAL_UNIT_ASSIGNED_CONTEXT((#11917,#11919,#11920))
REPRESENTATION_CONTEXT('','3D')
);
#11876=(
GEOMETRIC_REPRESENTATION_CONTEXT(3)
GLOBAL_UNCERTAINTY_ASSIGNED_CONTEXT((#11829))
GLOBAL_UNIT_ASSIGNED_CONTEXT((#11917,#11919,#11920))
REPRESENTATION_CONTEXT('','3D')
);
#11877=(
GEOMETRIC_REPRESENTATION_CONTEXT(3)
GLOBAL_UNCERTAINTY_ASSIGNED_CONTEXT((#11830))
GLOBAL_UNIT_ASSIGNED_CONTEXT((#11917,#11919,#11920))
REPRESENTATION_CONTEXT('','3D')
);
#11878=(
GEOMETRIC_REPRESENTATION_CONTEXT(3)
GLOBAL_UNCERTAINTY_ASSIGNED_CONTEXT((#11831))
GLOBAL_UNIT_ASSIGNED_CONTEXT((#11917,#11919,#11920))
REPRESENTATION_CONTEXT('','3D')
);
#11879=(
GEOMETRIC_REPRESENTATION_CONTEXT(3)
GLOBAL_UNCERTAINTY_ASSIGNED_CONTEXT((#11832))
GLOBAL_UNIT_ASSIGNED_CONTEXT((#11917,#11919,#11920))
REPRESENTATION_CONTEXT('','3D')
);
#11880=(
GEOMETRIC_REPRESENTATION_CONTEXT(3)
GLOBAL_UNCERTAINTY_ASSIGNED_CONTEXT((#11833))
GLOBAL_UNIT_ASSIGNED_CONTEXT((#11917,#11919,#11920))
REPRESENTATION_CONTEXT('','3D')
);
#11881=(
GEOMETRIC_REPRESENTATION_CONTEXT(3)
GLOBAL_UNCERTAINTY_ASSIGNED_CONTEXT((#11834))
GLOBAL_UNIT_ASSIGNED_CONTEXT((#11917,#11919,#11920))
REPRESENTATION_CONTEXT('','3D')
);
#11882=(
GEOMETRIC_REPRESENTATION_CONTEXT(3)
GLOBAL_UNCERTAINTY_ASSIGNED_CONTEXT((#11835))
GLOBAL_UNIT_ASSIGNED_CONTEXT((#11917,#11919,#11920))
REPRESENTATION_CONTEXT('','3D')
);
#11883=(
GEOMETRIC_REPRESENTATION_CONTEXT(3)
GLOBAL_UNCERTAINTY_ASSIGNED_CONTEXT((#11836))
GLOBAL_UNIT_ASSIGNED_CONTEXT((#11917,#11919,#11920))
REPRESENTATION_CONTEXT('','3D')
);
#11884=(
GEOMETRIC_REPRESENTATION_CONTEXT(3)
GLOBAL_UNCERTAINTY_ASSIGNED_CONTEXT((#11837))
GLOBAL_UNIT_ASSIGNED_CONTEXT((#11917,#11919,#11920))
REPRESENTATION_CONTEXT('','3D')
);
#11885=(
GEOMETRIC_REPRESENTATION_CONTEXT(3)
GLOBAL_UNCERTAINTY_ASSIGNED_CONTEXT((#11838))
GLOBAL_UNIT_ASSIGNED_CONTEXT((#11917,#11919,#11920))
REPRESENTATION_CONTEXT('','3D')
);
#11886=(
GEOMETRIC_REPRESENTATION_CONTEXT(3)
GLOBAL_UNCERTAINTY_ASSIGNED_CONTEXT((#11839))
GLOBAL_UNIT_ASSIGNED_CONTEXT((#11917,#11919,#11920))
REPRESENTATION_CONTEXT('','3D')
);
#11887=(
GEOMETRIC_REPRESENTATION_CONTEXT(3)
GLOBAL_UNCERTAINTY_ASSIGNED_CONTEXT((#11840))
GLOBAL_UNIT_ASSIGNED_CONTEXT((#11917,#11919,#11920))
REPRESENTATION_CONTEXT('','3D')
);
#11888=(
GEOMETRIC_REPRESENTATION_CONTEXT(3)
GLOBAL_UNCERTAINTY_ASSIGNED_CONTEXT((#11841))
GLOBAL_UNIT_ASSIGNED_CONTEXT((#11917,#11919,#11920))
REPRESENTATION_CONTEXT('','3D')
);
#11889=(
GEOMETRIC_REPRESENTATION_CONTEXT(3)
GLOBAL_UNCERTAINTY_ASSIGNED_CONTEXT((#11842))
GLOBAL_UNIT_ASSIGNED_CONTEXT((#11917,#11919,#11920))
REPRESENTATION_CONTEXT('','3D')
);
#11890=(
GEOMETRIC_REPRESENTATION_CONTEXT(3)
GLOBAL_UNCERTAINTY_ASSIGNED_CONTEXT((#11843))
GLOBAL_UNIT_ASSIGNED_CONTEXT((#11917,#11919,#11920))
REPRESENTATION_CONTEXT('','3D')
);
#11891=(
GEOMETRIC_REPRESENTATION_CONTEXT(3)
GLOBAL_UNCERTAINTY_ASSIGNED_CONTEXT((#11844))
GLOBAL_UNIT_ASSIGNED_CONTEXT((#11917,#11919,#11920))
REPRESENTATION_CONTEXT('','3D')
);
#11892=(
GEOMETRIC_REPRESENTATION_CONTEXT(3)
GLOBAL_UNCERTAINTY_ASSIGNED_CONTEXT((#11845))
GLOBAL_UNIT_ASSIGNED_CONTEXT((#11917,#11919,#11920))
REPRESENTATION_CONTEXT('','3D')
);
#11893=(
GEOMETRIC_REPRESENTATION_CONTEXT(3)
GLOBAL_UNCERTAINTY_ASSIGNED_CONTEXT((#11846))
GLOBAL_UNIT_ASSIGNED_CONTEXT((#11917,#11919,#11920))
REPRESENTATION_CONTEXT('','3D')
);
#11894=(
GEOMETRIC_REPRESENTATION_CONTEXT(3)
GLOBAL_UNCERTAINTY_ASSIGNED_CONTEXT((#11847))
GLOBAL_UNIT_ASSIGNED_CONTEXT((#11917,#11919,#11920))
REPRESENTATION_CONTEXT('','3D')
);
#11895=(
GEOMETRIC_REPRESENTATION_CONTEXT(3)
GLOBAL_UNCERTAINTY_ASSIGNED_CONTEXT((#11848))
GLOBAL_UNIT_ASSIGNED_CONTEXT((#11917,#11919,#11920))
REPRESENTATION_CONTEXT('','3D')
);
#11896=(
GEOMETRIC_REPRESENTATION_CONTEXT(3)
GLOBAL_UNCERTAINTY_ASSIGNED_CONTEXT((#11849))
GLOBAL_UNIT_ASSIGNED_CONTEXT((#11917,#11919,#11920))
REPRESENTATION_CONTEXT('','3D')
);
#11897=(
GEOMETRIC_REPRESENTATION_CONTEXT(3)
GLOBAL_UNCERTAINTY_ASSIGNED_CONTEXT((#11850))
GLOBAL_UNIT_ASSIGNED_CONTEXT((#11917,#11919,#11920))
REPRESENTATION_CONTEXT('','3D')
);
#11898=(
GEOMETRIC_REPRESENTATION_CONTEXT(3)
GLOBAL_UNCERTAINTY_ASSIGNED_CONTEXT((#11851))
GLOBAL_UNIT_ASSIGNED_CONTEXT((#11917,#11919,#11920))
REPRESENTATION_CONTEXT('','3D')
);
#11899=(
GEOMETRIC_REPRESENTATION_CONTEXT(3)
GLOBAL_UNCERTAINTY_ASSIGNED_CONTEXT((#11852))
GLOBAL_UNIT_ASSIGNED_CONTEXT((#11917,#11919,#11920))
REPRESENTATION_CONTEXT('','3D')
);
#11900=(
GEOMETRIC_REPRESENTATION_CONTEXT(3)
GLOBAL_UNCERTAINTY_ASSIGNED_CONTEXT((#11853))
GLOBAL_UNIT_ASSIGNED_CONTEXT((#11917,#11919,#11920))
REPRESENTATION_CONTEXT('','3D')
);
#11901=(
GEOMETRIC_REPRESENTATION_CONTEXT(3)
GLOBAL_UNCERTAINTY_ASSIGNED_CONTEXT((#11854))
GLOBAL_UNIT_ASSIGNED_CONTEXT((#11917,#11919,#11920))
REPRESENTATION_CONTEXT('','3D')
);
#11902=(
GEOMETRIC_REPRESENTATION_CONTEXT(3)
GLOBAL_UNCERTAINTY_ASSIGNED_CONTEXT((#11855))
GLOBAL_UNIT_ASSIGNED_CONTEXT((#11917,#11919,#11920))
REPRESENTATION_CONTEXT('','3D')
);
#11903=(
GEOMETRIC_REPRESENTATION_CONTEXT(3)
GLOBAL_UNCERTAINTY_ASSIGNED_CONTEXT((#11856))
GLOBAL_UNIT_ASSIGNED_CONTEXT((#11917,#11919,#11920))
REPRESENTATION_CONTEXT('','3D')
);
#11904=(
GEOMETRIC_REPRESENTATION_CONTEXT(3)
GLOBAL_UNCERTAINTY_ASSIGNED_CONTEXT((#11857))
GLOBAL_UNIT_ASSIGNED_CONTEXT((#11917,#11919,#11920))
REPRESENTATION_CONTEXT('','3D')
);
#11905=(
GEOMETRIC_REPRESENTATION_CONTEXT(3)
GLOBAL_UNCERTAINTY_ASSIGNED_CONTEXT((#11858))
GLOBAL_UNIT_ASSIGNED_CONTEXT((#11917,#11919,#11920))
REPRESENTATION_CONTEXT('','3D')
);
#11906=(
GEOMETRIC_REPRESENTATION_CONTEXT(3)
GLOBAL_UNCERTAINTY_ASSIGNED_CONTEXT((#11859))
GLOBAL_UNIT_ASSIGNED_CONTEXT((#11917,#11919,#11920))
REPRESENTATION_CONTEXT('','3D')
);
#11907=(
GEOMETRIC_REPRESENTATION_CONTEXT(3)
GLOBAL_UNCERTAINTY_ASSIGNED_CONTEXT((#11860))
GLOBAL_UNIT_ASSIGNED_CONTEXT((#11917,#11919,#11920))
REPRESENTATION_CONTEXT('','3D')
);
#11908=(
GEOMETRIC_REPRESENTATION_CONTEXT(3)
GLOBAL_UNCERTAINTY_ASSIGNED_CONTEXT((#11861))
GLOBAL_UNIT_ASSIGNED_CONTEXT((#11917,#11919,#11920))
REPRESENTATION_CONTEXT('','3D')
);
#11909=(
GEOMETRIC_REPRESENTATION_CONTEXT(3)
GLOBAL_UNCERTAINTY_ASSIGNED_CONTEXT((#11862))
GLOBAL_UNIT_ASSIGNED_CONTEXT((#11917,#11919,#11920))
REPRESENTATION_CONTEXT('','3D')
);
#11910=(
GEOMETRIC_REPRESENTATION_CONTEXT(3)
GLOBAL_UNCERTAINTY_ASSIGNED_CONTEXT((#11863))
GLOBAL_UNIT_ASSIGNED_CONTEXT((#11917,#11919,#11920))
REPRESENTATION_CONTEXT('','3D')
);
#11911=(
GEOMETRIC_REPRESENTATION_CONTEXT(3)
GLOBAL_UNCERTAINTY_ASSIGNED_CONTEXT((#11864))
GLOBAL_UNIT_ASSIGNED_CONTEXT((#11917,#11919,#11920))
REPRESENTATION_CONTEXT('','3D')
);
#11912=(
GEOMETRIC_REPRESENTATION_CONTEXT(3)
GLOBAL_UNCERTAINTY_ASSIGNED_CONTEXT((#11865))
GLOBAL_UNIT_ASSIGNED_CONTEXT((#11917,#11919,#11920))
REPRESENTATION_CONTEXT('','3D')
);
#11913=(
GEOMETRIC_REPRESENTATION_CONTEXT(3)
GLOBAL_UNCERTAINTY_ASSIGNED_CONTEXT((#11866))
GLOBAL_UNIT_ASSIGNED_CONTEXT((#11917,#11919,#11920))
REPRESENTATION_CONTEXT('','3D')
);
#11914=(
GEOMETRIC_REPRESENTATION_CONTEXT(3)
GLOBAL_UNCERTAINTY_ASSIGNED_CONTEXT((#11867))
GLOBAL_UNIT_ASSIGNED_CONTEXT((#11917,#11919,#11920))
REPRESENTATION_CONTEXT('','3D')
);
#11915=(
GEOMETRIC_REPRESENTATION_CONTEXT(3)
GLOBAL_UNCERTAINTY_ASSIGNED_CONTEXT((#11868))
GLOBAL_UNIT_ASSIGNED_CONTEXT((#11917,#11919,#11920))
REPRESENTATION_CONTEXT('','3D')
);
#11916=(
GEOMETRIC_REPRESENTATION_CONTEXT(3)
GLOBAL_UNCERTAINTY_ASSIGNED_CONTEXT((#11869))
GLOBAL_UNIT_ASSIGNED_CONTEXT((#11917,#11919,#11920))
REPRESENTATION_CONTEXT('','3D')
);
#11917=(
LENGTH_UNIT()
NAMED_UNIT(*)
SI_UNIT(.CENTI.,.METRE.)
);
#11918=(
LENGTH_UNIT()
NAMED_UNIT(*)
SI_UNIT($,.METRE.)
);
#11919=(
NAMED_UNIT(*)
PLANE_ANGLE_UNIT()
SI_UNIT($,.RADIAN.)
);
#11920=(
NAMED_UNIT(*)
SI_UNIT($,.STERADIAN.)
SOLID_ANGLE_UNIT()
);
#11921=SHAPE_DEFINITION_REPRESENTATION(#11967,#12079);
#11922=SHAPE_DEFINITION_REPRESENTATION(#11968,#12080);
#11923=SHAPE_DEFINITION_REPRESENTATION(#11969,#12081);
#11924=SHAPE_DEFINITION_REPRESENTATION(#11970,#12082);
#11925=SHAPE_DEFINITION_REPRESENTATION(#11971,#12083);
#11926=SHAPE_DEFINITION_REPRESENTATION(#11972,#12084);
#11927=SHAPE_DEFINITION_REPRESENTATION(#11973,#12085);
#11928=SHAPE_DEFINITION_REPRESENTATION(#11974,#12086);
#11929=SHAPE_DEFINITION_REPRESENTATION(#11975,#12087);
#11930=SHAPE_DEFINITION_REPRESENTATION(#11976,#12088);
#11931=SHAPE_DEFINITION_REPRESENTATION(#11977,#12089);
#11932=SHAPE_DEFINITION_REPRESENTATION(#11978,#12090);
#11933=SHAPE_DEFINITION_REPRESENTATION(#11979,#12091);
#11934=SHAPE_DEFINITION_REPRESENTATION(#11980,#12092);
#11935=SHAPE_DEFINITION_REPRESENTATION(#11981,#12093);
#11936=SHAPE_DEFINITION_REPRESENTATION(#11982,#12094);
#11937=SHAPE_DEFINITION_REPRESENTATION(#11983,#12095);
#11938=SHAPE_DEFINITION_REPRESENTATION(#11989,#12096);
#11939=SHAPE_DEFINITION_REPRESENTATION(#11990,#12097);
#11940=SHAPE_DEFINITION_REPRESENTATION(#11991,#12098);
#11941=SHAPE_DEFINITION_REPRESENTATION(#11992,#12099);
#11942=SHAPE_DEFINITION_REPRESENTATION(#11993,#12100);
#11943=SHAPE_DEFINITION_REPRESENTATION(#11994,#12101);
#11944=SHAPE_DEFINITION_REPRESENTATION(#11995,#12102);
#11945=SHAPE_DEFINITION_REPRESENTATION(#11996,#12103);
#11946=SHAPE_DEFINITION_REPRESENTATION(#11997,#12104);
#11947=SHAPE_DEFINITION_REPRESENTATION(#11998,#12105);
#11948=SHAPE_DEFINITION_REPRESENTATION(#11999,#12106);
#11949=SHAPE_DEFINITION_REPRESENTATION(#12000,#12107);
#11950=SHAPE_DEFINITION_REPRESENTATION(#12001,#12108);
#11951=SHAPE_DEFINITION_REPRESENTATION(#12002,#12109);
#11952=SHAPE_DEFINITION_REPRESENTATION(#12003,#12110);
#11953=SHAPE_DEFINITION_REPRESENTATION(#12004,#12111);
#11954=SHAPE_DEFINITION_REPRESENTATION(#12005,#12112);
#11955=SHAPE_DEFINITION_REPRESENTATION(#12006,#12113);
#11956=SHAPE_DEFINITION_REPRESENTATION(#12007,#12114);
#11957=SHAPE_DEFINITION_REPRESENTATION(#12008,#12115);
#11958=SHAPE_DEFINITION_REPRESENTATION(#12009,#12116);
#11959=SHAPE_DEFINITION_REPRESENTATION(#12010,#12117);
#11960=SHAPE_DEFINITION_REPRESENTATION(#12011,#12118);
#11961=SHAPE_DEFINITION_REPRESENTATION(#12012,#12119);
#11962=SHAPE_DEFINITION_REPRESENTATION(#12013,#12120);
#11963=SHAPE_DEFINITION_REPRESENTATION(#12068,#12121);
#11964=SHAPE_DEFINITION_REPRESENTATION(#12069,#12122);
#11965=SHAPE_DEFINITION_REPRESENTATION(#12070,#12123);
#11966=SHAPE_DEFINITION_REPRESENTATION(#12071,#12124);
#11967=PRODUCT_DEFINITION_SHAPE('',$,#12126);
#11968=PRODUCT_DEFINITION_SHAPE('',$,#12127);
#11969=PRODUCT_DEFINITION_SHAPE('',$,#12128);
#11970=PRODUCT_DEFINITION_SHAPE('',$,#12129);
#11971=PRODUCT_DEFINITION_SHAPE('',$,#12130);
#11972=PRODUCT_DEFINITION_SHAPE('',$,#12131);
#11973=PRODUCT_DEFINITION_SHAPE('',$,#12132);
#11974=PRODUCT_DEFINITION_SHAPE('',$,#12133);
#11975=PRODUCT_DEFINITION_SHAPE('',$,#12134);
#11976=PRODUCT_DEFINITION_SHAPE('',$,#12135);
#11977=PRODUCT_DEFINITION_SHAPE('',$,#12136);
#11978=PRODUCT_DEFINITION_SHAPE('',$,#12137);
#11979=PRODUCT_DEFINITION_SHAPE('',$,#12138);
#11980=PRODUCT_DEFINITION_SHAPE('',$,#12139);
#11981=PRODUCT_DEFINITION_SHAPE('',$,#12140);
#11982=PRODUCT_DEFINITION_SHAPE('',$,#12141);
#11983=PRODUCT_DEFINITION_SHAPE('',$,#12142);
#11984=PRODUCT_DEFINITION_SHAPE($,$,#209);
#11985=PRODUCT_DEFINITION_SHAPE($,$,#210);
#11986=PRODUCT_DEFINITION_SHAPE($,$,#211);
#11987=PRODUCT_DEFINITION_SHAPE($,$,#212);
#11988=PRODUCT_DEFINITION_SHAPE($,$,#213);
#11989=PRODUCT_DEFINITION_SHAPE('',$,#12143);
#11990=PRODUCT_DEFINITION_SHAPE('',$,#12144);
#11991=PRODUCT_DEFINITION_SHAPE('',$,#12145);
#11992=PRODUCT_DEFINITION_SHAPE('',$,#12146);
#11993=PRODUCT_DEFINITION_SHAPE('',$,#12147);
#11994=PRODUCT_DEFINITION_SHAPE('',$,#12148);
#11995=PRODUCT_DEFINITION_SHAPE('',$,#12149);
#11996=PRODUCT_DEFINITION_SHAPE('',$,#12150);
#11997=PRODUCT_DEFINITION_SHAPE('',$,#12151);
#11998=PRODUCT_DEFINITION_SHAPE('',$,#12152);
#11999=PRODUCT_DEFINITION_SHAPE('',$,#12153);
#12000=PRODUCT_DEFINITION_SHAPE('',$,#12154);
#12001=PRODUCT_DEFINITION_SHAPE('',$,#12155);
#12002=PRODUCT_DEFINITION_SHAPE('',$,#12156);
#12003=PRODUCT_DEFINITION_SHAPE('',$,#12157);
#12004=PRODUCT_DEFINITION_SHAPE('',$,#12158);
#12005=PRODUCT_DEFINITION_SHAPE('',$,#12159);
#12006=PRODUCT_DEFINITION_SHAPE('',$,#12160);
#12007=PRODUCT_DEFINITION_SHAPE('',$,#12161);
#12008=PRODUCT_DEFINITION_SHAPE('',$,#12162);
#12009=PRODUCT_DEFINITION_SHAPE('',$,#12163);
#12010=PRODUCT_DEFINITION_SHAPE('',$,#12164);
#12011=PRODUCT_DEFINITION_SHAPE('',$,#12165);
#12012=PRODUCT_DEFINITION_SHAPE('',$,#12166);
#12013=PRODUCT_DEFINITION_SHAPE('',$,#12167);
#12014=PRODUCT_DEFINITION_SHAPE($,$,#214);
#12015=PRODUCT_DEFINITION_SHAPE($,$,#215);
#12016=PRODUCT_DEFINITION_SHAPE($,$,#216);
#12017=PRODUCT_DEFINITION_SHAPE($,$,#217);
#12018=PRODUCT_DEFINITION_SHAPE($,$,#218);
#12019=PRODUCT_DEFINITION_SHAPE($,$,#219);
#12020=PRODUCT_DEFINITION_SHAPE($,$,#220);
#12021=PRODUCT_DEFINITION_SHAPE($,$,#221);
#12022=PRODUCT_DEFINITION_SHAPE($,$,#222);
#12023=PRODUCT_DEFINITION_SHAPE($,$,#223);
#12024=PRODUCT_DEFINITION_SHAPE($,$,#224);
#12025=PRODUCT_DEFINITION_SHAPE($,$,#225);
#12026=PRODUCT_DEFINITION_SHAPE($,$,#226);
#12027=PRODUCT_DEFINITION_SHAPE($,$,#227);
#12028=PRODUCT_DEFINITION_SHAPE($,$,#228);
#12029=PRODUCT_DEFINITION_SHAPE($,$,#229);
#12030=PRODUCT_DEFINITION_SHAPE($,$,#230);
#12031=PRODUCT_DEFINITION_SHAPE($,$,#231);
#12032=PRODUCT_DEFINITION_SHAPE($,$,#232);
#12033=PRODUCT_DEFINITION_SHAPE($,$,#233);
#12034=PRODUCT_DEFINITION_SHAPE($,$,#234);
#12035=PRODUCT_DEFINITION_SHAPE($,$,#235);
#12036=PRODUCT_DEFINITION_SHAPE($,$,#236);
#12037=PRODUCT_DEFINITION_SHAPE($,$,#237);
#12038=PRODUCT_DEFINITION_SHAPE($,$,#238);
#12039=PRODUCT_DEFINITION_SHAPE($,$,#239);
#12040=PRODUCT_DEFINITION_SHAPE($,$,#240);
#12041=PRODUCT_DEFINITION_SHAPE($,$,#241);
#12042=PRODUCT_DEFINITION_SHAPE($,$,#242);
#12043=PRODUCT_DEFINITION_SHAPE($,$,#243);
#12044=PRODUCT_DEFINITION_SHAPE($,$,#244);
#12045=PRODUCT_DEFINITION_SHAPE($,$,#245);
#12046=PRODUCT_DEFINITION_SHAPE($,$,#246);
#12047=PRODUCT_DEFINITION_SHAPE($,$,#247);
#12048=PRODUCT_DEFINITION_SHAPE($,$,#248);
#12049=PRODUCT_DEFINITION_SHAPE($,$,#249);
#12050=PRODUCT_DEFINITION_SHAPE($,$,#250);
#12051=PRODUCT_DEFINITION_SHAPE($,$,#251);
#12052=PRODUCT_DEFINITION_SHAPE($,$,#252);
#12053=PRODUCT_DEFINITION_SHAPE($,$,#253);
#12054=PRODUCT_DEFINITION_SHAPE($,$,#254);
#12055=PRODUCT_DEFINITION_SHAPE($,$,#255);
#12056=PRODUCT_DEFINITION_SHAPE($,$,#256);
#12057=PRODUCT_DEFINITION_SHAPE($,$,#257);
#12058=PRODUCT_DEFINITION_SHAPE($,$,#258);
#12059=PRODUCT_DEFINITION_SHAPE($,$,#259);
#12060=PRODUCT_DEFINITION_SHAPE($,$,#260);
#12061=PRODUCT_DEFINITION_SHAPE($,$,#261);
#12062=PRODUCT_DEFINITION_SHAPE($,$,#262);
#12063=PRODUCT_DEFINITION_SHAPE($,$,#263);
#12064=PRODUCT_DEFINITION_SHAPE($,$,#264);
#12065=PRODUCT_DEFINITION_SHAPE($,$,#265);
#12066=PRODUCT_DEFINITION_SHAPE($,$,#266);
#12067=PRODUCT_DEFINITION_SHAPE($,$,#267);
#12068=PRODUCT_DEFINITION_SHAPE('',$,#12168);
#12069=PRODUCT_DEFINITION_SHAPE('',$,#12169);
#12070=PRODUCT_DEFINITION_SHAPE('',$,#12170);
#12071=PRODUCT_DEFINITION_SHAPE('',$,#12171);
#12072=PRODUCT_DEFINITION_SHAPE($,$,#268);
#12073=PRODUCT_DEFINITION_SHAPE($,$,#269);
#12074=PRODUCT_DEFINITION_SHAPE($,$,#270);
#12075=PRODUCT_DEFINITION_SHAPE($,$,#271);
#12076=PRODUCT_DEFINITION_SHAPE($,$,#272);
#12077=PRODUCT_DEFINITION_SHAPE($,$,#273);
#12078=PRODUCT_DEFINITION_SHAPE($,$,#274);
#12079=SHAPE_REPRESENTATION('',(#6559,#7407,#7408,#7409,#7410),#11870);
#12080=SHAPE_REPRESENTATION('',(#6560,#7314,#7315,#7316,#7317,#7318,#7319,
#7320,#7321,#7322,#7323,#7324,#7325,#7326,#7327,#7328,#7329,#7330,#7331,
#7332,#7333,#7334,#7335,#7336,#7337,#7338,#7339,#7340),#11871);
#12081=SHAPE_REPRESENTATION('',(#6561),#11872);
#12082=SHAPE_REPRESENTATION('',(#6592),#11873);
#12083=SHAPE_REPRESENTATION('',(#6599),#11874);
#12084=SHAPE_REPRESENTATION('',(#6606),#11875);
#12085=SHAPE_REPRESENTATION('',(#6676),#11876);
#12086=SHAPE_REPRESENTATION('',(#6685),#11877);
#12087=SHAPE_REPRESENTATION('',(#6710),#11878);
#12088=SHAPE_REPRESENTATION('',(#6780),#11879);
#12089=SHAPE_REPRESENTATION('',(#6805),#11880);
#12090=SHAPE_REPRESENTATION('',(#6829,#6958,#6959,#6960,#6961,#6962),#11881);
#12091=SHAPE_REPRESENTATION('',(#6830),#11882);
#12092=SHAPE_REPRESENTATION('',(#6850),#11883);
#12093=SHAPE_REPRESENTATION('',(#6870),#11884);
#12094=SHAPE_REPRESENTATION('',(#6887),#11885);
#12095=SHAPE_REPRESENTATION('',(#6941),#11886);
#12096=SHAPE_REPRESENTATION('',(#6963,#7341,#7342,#7343,#7344,#7345,#7346,
#7347,#7348,#7349,#7350,#7351,#7352,#7353,#7354,#7355,#7356),#11887);
#12097=SHAPE_REPRESENTATION('',(#6964),#11888);
#12098=SHAPE_REPRESENTATION('',(#6994),#11889);
#12099=SHAPE_REPRESENTATION('',(#7003),#11890);
#12100=SHAPE_REPRESENTATION('',(#7012),#11891);
#12101=SHAPE_REPRESENTATION('',(#7026),#11892);
#12102=SHAPE_REPRESENTATION('',(#7040),#11893);
#12103=SHAPE_REPRESENTATION('',(#7049),#11894);
#12104=SHAPE_REPRESENTATION('',(#7071),#11895);
#12105=SHAPE_REPRESENTATION('',(#7080),#11896);
#12106=SHAPE_REPRESENTATION('',(#7089),#11897);
#12107=SHAPE_REPRESENTATION('',(#7098),#11898);
#12108=SHAPE_REPRESENTATION('',(#7107),#11899);
#12109=SHAPE_REPRESENTATION('',(#7124,#7357,#7358,#7359,#7360,#7361,#7362,
#7363,#7364,#7365,#7366,#7367),#11900);
#12110=SHAPE_REPRESENTATION('',(#7125),#11901);
#12111=SHAPE_REPRESENTATION('',(#7168),#11902);
#12112=SHAPE_REPRESENTATION('',(#7177),#11903);
#12113=SHAPE_REPRESENTATION('',(#7191),#11904);
#12114=SHAPE_REPRESENTATION('',(#7213),#11905);
#12115=SHAPE_REPRESENTATION('',(#7222),#11906);
#12116=SHAPE_REPRESENTATION('',(#7231),#11907);
#12117=SHAPE_REPRESENTATION('',(#7240),#11908);
#12118=SHAPE_REPRESENTATION('',(#7249),#11909);
#12119=SHAPE_REPRESENTATION('',(#7264),#11910);
#12120=SHAPE_REPRESENTATION('',(#7290),#11911);
#12121=SHAPE_REPRESENTATION('',(#7368,#7404,#7405,#7406),#11912);
#12122=SHAPE_REPRESENTATION('',(#7369),#11913);
#12123=SHAPE_REPRESENTATION('',(#7386),#11914);
#12124=SHAPE_REPRESENTATION('',(#7395),#11915);
#12125=PRODUCT_DEFINITION_CONTEXT('part definition',#12265,'design');
#12126=PRODUCT_DEFINITION(
'PAT-027','PAT-027',#12172,
#12125);
#12127=PRODUCT_DEFINITION('Bearing base','Bearing base',#12173,#12125);
#12128=PRODUCT_DEFINITION('Base','Base',#12174,#12125);
#12129=PRODUCT_DEFINITION('Foot strip','Foot strip',#12175,#12125);
#12130=PRODUCT_DEFINITION('Foot strip (1)','Foot strip (1)',#12176,#12125);
#12131=PRODUCT_DEFINITION('Input pedestal','Input pedestal',#12177,#12125);
#12132=PRODUCT_DEFINITION('Input outer spacer','Input outer spacer',#12178,
#12125);
#12133=PRODUCT_DEFINITION('Input cap','Input cap',#12179,#12125);
#12134=PRODUCT_DEFINITION('Output pedestal','Output pedestal',#12180,#12125);
#12135=PRODUCT_DEFINITION('Output cap','Output cap',#12181,#12125);
#12136=PRODUCT_DEFINITION('M5x14 Cap Screw','M5x14 Cap Screw',#12182,#12125);
#12137=PRODUCT_DEFINITION('Sealed Ball Bearing - 10 x 30 x 9 mm',
'Sealed Ball Bearing - 10 x 30 x 9 mm',#12183,#12125);
#12138=PRODUCT_DEFINITION('Inner ring','Inner ring',#12184,#12125);
#12139=PRODUCT_DEFINITION('Outer ring','Outer ring',#12185,#12125);
#12140=PRODUCT_DEFINITION('Balls','Balls',#12186,#12125);
#12141=PRODUCT_DEFINITION('Cage','Cage',#12187,#12125);
#12142=PRODUCT_DEFINITION('Seals 2RS','Seals 2RS',#12188,#12125);
#12143=PRODUCT_DEFINITION('Continuous input crank',
'Continuous input crank',#12189,#12125);
#12144=PRODUCT_DEFINITION('Input crank and shaft',
'Input crank and shaft',#12190,#12125);
#12145=PRODUCT_DEFINITION('Input inner sleeve','Input inner sleeve',#12191,
#12125);
#12146=PRODUCT_DEFINITION('Intermediate inner sleeve',
'Intermediate inner sleeve',#12192,#12125);
#12147=PRODUCT_DEFINITION('Shaft collar','Shaft collar',#12193,#12125);
#12148=PRODUCT_DEFINITION('Input knob','Input knob',#12194,#12125);
#12149=PRODUCT_DEFINITION('Knob keeper','Knob keeper',#12195,#12125);
#12150=PRODUCT_DEFINITION('Link pin','Link pin',#12196,#12125);
#12151=PRODUCT_DEFINITION('Rear link spacer','Rear link spacer',#12197,
#12125);
#12152=PRODUCT_DEFINITION('Front link spacer','Front link spacer',#12198,
#12125);
#12153=PRODUCT_DEFINITION('Lower pin keeper','Lower pin keeper',#12199,
#12125);
#12154=PRODUCT_DEFINITION('Upper pin keeper','Upper pin keeper',#12200,
#12125);
#12155=PRODUCT_DEFINITION('Socket Set Screw - M4x6',
'Socket Set Screw - M4x6',#12201,#12125);
#12156=PRODUCT_DEFINITION('Oscillating output post',
'Oscillating output post',#12202,#12125);
#12157=PRODUCT_DEFINITION('Output rocker and post',
'Output rocker and post',#12203,#12125);
#12158=PRODUCT_DEFINITION('Output inner sleeve','Output inner sleeve',#12204,
#12125);
#12159=PRODUCT_DEFINITION('Shaft collar (1)','Shaft collar (1)',#12205,#12125);
#12160=PRODUCT_DEFINITION('Link pin (1)','Link pin (1)',#12206,#12125);
#12161=PRODUCT_DEFINITION('Rear link spacer (1)','Rear link spacer (1)',#12207,
#12125);
#12162=PRODUCT_DEFINITION('Front link spacer (1)','Front link spacer (1)',
#12208,#12125);
#12163=PRODUCT_DEFINITION('Lower pin keeper (1)','Lower pin keeper (1)',#12209,
#12125);
#12164=PRODUCT_DEFINITION('Upper pin keeper (1)','Upper pin keeper (1)',#12210,
#12125);
#12165=PRODUCT_DEFINITION('M4x4 collar screw','M4x4 collar screw',#12211,
#12125);
#12166=PRODUCT_DEFINITION('Cap Screw - M4x16','Cap Screw - M4x16',#12212,
#12125);
#12167=PRODUCT_DEFINITION('M4x10 Cap Screw','M4x10 Cap Screw',#12213,#12125);
#12168=PRODUCT_DEFINITION('Connecting link (1)','Connecting link (1)',#12214,
#12125);
#12169=PRODUCT_DEFINITION('Connecting link','Connecting link',#12215,
#12125);
#12170=PRODUCT_DEFINITION('Link bushing','Link bushing',#12216,#12125);
#12171=PRODUCT_DEFINITION('Link bushing (1)','Link bushing (1)',#12217,#12125);
#12172=PRODUCT_DEFINITION_FORMATION('',$,#12267);
#12173=PRODUCT_DEFINITION_FORMATION('',$,#12268);
#12174=PRODUCT_DEFINITION_FORMATION('',$,#12269);
#12175=PRODUCT_DEFINITION_FORMATION('',$,#12270);
#12176=PRODUCT_DEFINITION_FORMATION('',$,#12271);
#12177=PRODUCT_DEFINITION_FORMATION('',$,#12272);
#12178=PRODUCT_DEFINITION_FORMATION('',$,#12273);
#12179=PRODUCT_DEFINITION_FORMATION('',$,#12274);
#12180=PRODUCT_DEFINITION_FORMATION('',$,#12275);
#12181=PRODUCT_DEFINITION_FORMATION('',$,#12276);
#12182=PRODUCT_DEFINITION_FORMATION('',$,#12277);
#12183=PRODUCT_DEFINITION_FORMATION('',$,#12278);
#12184=PRODUCT_DEFINITION_FORMATION('',$,#12279);
#12185=PRODUCT_DEFINITION_FORMATION('',$,#12280);
#12186=PRODUCT_DEFINITION_FORMATION('',$,#12281);
#12187=PRODUCT_DEFINITION_FORMATION('',$,#12282);
#12188=PRODUCT_DEFINITION_FORMATION('',$,#12283);
#12189=PRODUCT_DEFINITION_FORMATION('',$,#12284);
#12190=PRODUCT_DEFINITION_FORMATION('',$,#12285);
#12191=PRODUCT_DEFINITION_FORMATION('',$,#12286);
#12192=PRODUCT_DEFINITION_FORMATION('',$,#12287);
#12193=PRODUCT_DEFINITION_FORMATION('',$,#12288);
#12194=PRODUCT_DEFINITION_FORMATION('',$,#12289);
#12195=PRODUCT_DEFINITION_FORMATION('',$,#12290);
#12196=PRODUCT_DEFINITION_FORMATION('',$,#12291);
#12197=PRODUCT_DEFINITION_FORMATION('',$,#12292);
#12198=PRODUCT_DEFINITION_FORMATION('',$,#12293);
#12199=PRODUCT_DEFINITION_FORMATION('',$,#12294);
#12200=PRODUCT_DEFINITION_FORMATION('',$,#12295);
#12201=PRODUCT_DEFINITION_FORMATION('',$,#12296);
#12202=PRODUCT_DEFINITION_FORMATION('',$,#12297);
#12203=PRODUCT_DEFINITION_FORMATION('',$,#12298);
#12204=PRODUCT_DEFINITION_FORMATION('',$,#12299);
#12205=PRODUCT_DEFINITION_FORMATION('',$,#12300);
#12206=PRODUCT_DEFINITION_FORMATION('',$,#12301);
#12207=PRODUCT_DEFINITION_FORMATION('',$,#12302);
#12208=PRODUCT_DEFINITION_FORMATION('',$,#12303);
#12209=PRODUCT_DEFINITION_FORMATION('',$,#12304);
#12210=PRODUCT_DEFINITION_FORMATION('',$,#12305);
#12211=PRODUCT_DEFINITION_FORMATION('',$,#12306);
#12212=PRODUCT_DEFINITION_FORMATION('',$,#12307);
#12213=PRODUCT_DEFINITION_FORMATION('',$,#12308);
#12214=PRODUCT_DEFINITION_FORMATION('',$,#12309);
#12215=PRODUCT_DEFINITION_FORMATION('',$,#12310);
#12216=PRODUCT_DEFINITION_FORMATION('',$,#12311);
#12217=PRODUCT_DEFINITION_FORMATION('',$,#12312);
#12218=PRODUCT_RELATED_PRODUCT_CATEGORY('PAT-027','PAT-027',(#12267));
#12219=PRODUCT_RELATED_PRODUCT_CATEGORY('Bearing base','Bearing base',(#12268));
#12220=PRODUCT_RELATED_PRODUCT_CATEGORY('Base','Base',(#12269));
#12221=PRODUCT_RELATED_PRODUCT_CATEGORY('Foot strip','Foot strip',(#12270));
#12222=PRODUCT_RELATED_PRODUCT_CATEGORY('Foot strip (1)',
'Foot strip (1)',(#12271));
#12223=PRODUCT_RELATED_PRODUCT_CATEGORY('Input pedestal',
'Input pedestal',(#12272));
#12224=PRODUCT_RELATED_PRODUCT_CATEGORY('Input outer spacer',
'Input outer spacer',(#12273));
#12225=PRODUCT_RELATED_PRODUCT_CATEGORY('Input cap','Input cap',(#12274));
#12226=PRODUCT_RELATED_PRODUCT_CATEGORY('Output pedestal',
'Output pedestal',(#12275));
#12227=PRODUCT_RELATED_PRODUCT_CATEGORY('Output cap','Output cap',(#12276));
#12228=PRODUCT_RELATED_PRODUCT_CATEGORY('M5x14 Cap Screw',
'M5x14 Cap Screw',(#12277));
#12229=PRODUCT_RELATED_PRODUCT_CATEGORY(
'Sealed Ball Bearing - 10 x 30 x 9 mm',
'Sealed Ball Bearing - 10 x 30 x 9 mm',(#12278));
#12230=PRODUCT_RELATED_PRODUCT_CATEGORY('Inner ring','Inner ring',(#12279));
#12231=PRODUCT_RELATED_PRODUCT_CATEGORY('Outer ring','Outer ring',(#12280));
#12232=PRODUCT_RELATED_PRODUCT_CATEGORY('Balls','Balls',(#12281));
#12233=PRODUCT_RELATED_PRODUCT_CATEGORY('Cage','Cage',(#12282));
#12234=PRODUCT_RELATED_PRODUCT_CATEGORY('Seals 2RS','Seals 2RS',(#12283));
#12235=PRODUCT_RELATED_PRODUCT_CATEGORY('Continuous input crank',
'Continuous input crank',(#12284));
#12236=PRODUCT_RELATED_PRODUCT_CATEGORY('Input crank and shaft',
'Input crank and shaft',(#12285));
#12237=PRODUCT_RELATED_PRODUCT_CATEGORY('Input inner sleeve',
'Input inner sleeve',(#12286));
#12238=PRODUCT_RELATED_PRODUCT_CATEGORY('Intermediate inner sleeve',
'Intermediate inner sleeve',(#12287));
#12239=PRODUCT_RELATED_PRODUCT_CATEGORY('Shaft collar','Shaft collar',(#12288));
#12240=PRODUCT_RELATED_PRODUCT_CATEGORY('Input knob','Input knob',(#12289));
#12241=PRODUCT_RELATED_PRODUCT_CATEGORY('Knob keeper','Knob keeper',(#12290));
#12242=PRODUCT_RELATED_PRODUCT_CATEGORY('Link pin','Link pin',(#12291));
#12243=PRODUCT_RELATED_PRODUCT_CATEGORY('Rear link spacer',
'Rear link spacer',(#12292));
#12244=PRODUCT_RELATED_PRODUCT_CATEGORY('Front link spacer',
'Front link spacer',(#12293));
#12245=PRODUCT_RELATED_PRODUCT_CATEGORY('Lower pin keeper',
'Lower pin keeper',(#12294));
#12246=PRODUCT_RELATED_PRODUCT_CATEGORY('Upper pin keeper',
'Upper pin keeper',(#12295));
#12247=PRODUCT_RELATED_PRODUCT_CATEGORY('Socket Set Screw - M4x6',
'Socket Set Screw - M4x6',(#12296));
#12248=PRODUCT_RELATED_PRODUCT_CATEGORY('Oscillating output post',
'Oscillating output post',(#12297));
#12249=PRODUCT_RELATED_PRODUCT_CATEGORY('Output rocker and post',
'Output rocker and post',(#12298));
#12250=PRODUCT_RELATED_PRODUCT_CATEGORY('Output inner sleeve',
'Output inner sleeve',(#12299));
#12251=PRODUCT_RELATED_PRODUCT_CATEGORY('Shaft collar (1)',
'Shaft collar (1)',(#12300));
#12252=PRODUCT_RELATED_PRODUCT_CATEGORY('Link pin (1)','Link pin (1)',(#12301));
#12253=PRODUCT_RELATED_PRODUCT_CATEGORY('Rear link spacer (1)',
'Rear link spacer (1)',(#12302));
#12254=PRODUCT_RELATED_PRODUCT_CATEGORY('Front link spacer (1)',
'Front link spacer (1)',(#12303));
#12255=PRODUCT_RELATED_PRODUCT_CATEGORY('Lower pin keeper (1)',
'Lower pin keeper (1)',(#12304));
#12256=PRODUCT_RELATED_PRODUCT_CATEGORY('Upper pin keeper (1)',
'Upper pin keeper (1)',(#12305));
#12257=PRODUCT_RELATED_PRODUCT_CATEGORY('M4x4 collar screw',
'M4x4 collar screw',(#12306));
#12258=PRODUCT_RELATED_PRODUCT_CATEGORY('Cap Screw - M4x16',
'Cap Screw - M4x16',(#12307));
#12259=PRODUCT_RELATED_PRODUCT_CATEGORY('M4x10 Cap Screw',
'M4x10 Cap Screw',(#12308));
#12260=PRODUCT_RELATED_PRODUCT_CATEGORY('Connecting link (1)',
'Connecting link (1)',(#12309));
#12261=PRODUCT_RELATED_PRODUCT_CATEGORY('Connecting link',
'Connecting link',(#12310));
#12262=PRODUCT_RELATED_PRODUCT_CATEGORY('Link bushing','Link bushing',(#12311));
#12263=PRODUCT_RELATED_PRODUCT_CATEGORY('Link bushing (1)',
'Link bushing (1)',(#12312));
#12264=APPLICATION_PROTOCOL_DEFINITION('international standard',
'automotive_design',2009,#12265);
#12265=APPLICATION_CONTEXT(
'Core Data for Automotive Mechanical Design Process');
#12266=PRODUCT_CONTEXT('part definition',#12265,'mechanical');
#12267=PRODUCT('PAT-027',
'PAT-027','PAT-027',(#12266));
#12268=PRODUCT('Bearing base','Bearing base','Bearing base',(#12266));
#12269=PRODUCT('Base','Base','Base',(#12266));
#12270=PRODUCT('Foot strip','Foot strip','Foot strip',(#12266));
#12271=PRODUCT('Foot strip (1)','Foot strip (1)','Foot strip (1)',(#12266));
#12272=PRODUCT('Input pedestal','Input pedestal','Input pedestal',(#12266));
#12273=PRODUCT('Input outer spacer','Input outer spacer',
'Input outer spacer',(#12266));
#12274=PRODUCT('Input cap','Input cap','Input cap',(#12266));
#12275=PRODUCT('Output pedestal','Output pedestal','Output pedestal',(#12266));
#12276=PRODUCT('Output cap','Output cap','Output cap',(#12266));
#12277=PRODUCT('M5x14 Cap Screw','M5x14 Cap Screw','M5x14 Cap Screw',(#12266));
#12278=PRODUCT('Sealed Ball Bearing - 10 x 30 x 9 mm',
'Sealed Ball Bearing - 10 x 30 x 9 mm',
'Sealed Ball Bearing - 10 x 30 x 9 mm',(#12266));
#12279=PRODUCT('Inner ring','Inner ring','Inner ring',(#12266));
#12280=PRODUCT('Outer ring','Outer ring','Outer ring',(#12266));
#12281=PRODUCT('Balls','Balls','Balls',(#12266));
#12282=PRODUCT('Cage','Cage','Cage',(#12266));
#12283=PRODUCT('Seals 2RS','Seals 2RS','Seals 2RS',(#12266));
#12284=PRODUCT('Continuous input crank','Continuous input crank',
'Continuous input crank',(#12266));
#12285=PRODUCT('Input crank and shaft','Input crank and shaft',
'Input crank and shaft',(#12266));
#12286=PRODUCT('Input inner sleeve','Input inner sleeve',
'Input inner sleeve',(#12266));
#12287=PRODUCT('Intermediate inner sleeve','Intermediate inner sleeve',
'Intermediate inner sleeve',(#12266));
#12288=PRODUCT('Shaft collar','Shaft collar','Shaft collar',(#12266));
#12289=PRODUCT('Input knob','Input knob','Input knob',(#12266));
#12290=PRODUCT('Knob keeper','Knob keeper','Knob keeper',(#12266));
#12291=PRODUCT('Link pin','Link pin','Link pin',(#12266));
#12292=PRODUCT('Rear link spacer','Rear link spacer','Rear link spacer',
(#12266));
#12293=PRODUCT('Front link spacer','Front link spacer',
'Front link spacer',(#12266));
#12294=PRODUCT('Lower pin keeper','Lower pin keeper','Lower pin keeper',
(#12266));
#12295=PRODUCT('Upper pin keeper','Upper pin keeper','Upper pin keeper',
(#12266));
#12296=PRODUCT('Socket Set Screw - M4x6','Socket Set Screw - M4x6',
'Socket Set Screw - M4x6',(#12266));
#12297=PRODUCT('Oscillating output post','Oscillating output post',
'Oscillating output post',(#12266));
#12298=PRODUCT('Output rocker and post','Output rocker and post',
'Output rocker and post',(#12266));
#12299=PRODUCT('Output inner sleeve','Output inner sleeve',
'Output inner sleeve',(#12266));
#12300=PRODUCT('Shaft collar (1)','Shaft collar (1)','Shaft collar (1)',(#12266));
#12301=PRODUCT('Link pin (1)','Link pin (1)','Link pin (1)',(#12266));
#12302=PRODUCT('Rear link spacer (1)','Rear link spacer (1)',
'Rear link spacer (1)',(#12266));
#12303=PRODUCT('Front link spacer (1)','Front link spacer (1)',
'Front link spacer (1)',(#12266));
#12304=PRODUCT('Lower pin keeper (1)','Lower pin keeper (1)',
'Lower pin keeper (1)',(#12266));
#12305=PRODUCT('Upper pin keeper (1)','Upper pin keeper (1)',
'Upper pin keeper (1)',(#12266));
#12306=PRODUCT('M4x4 collar screw','M4x4 collar screw',
'M4x4 collar screw',(#12266));
#12307=PRODUCT('Cap Screw - M4x16','Cap Screw - M4x16',
'Cap Screw - M4x16',(#12266));
#12308=PRODUCT('M4x10 Cap Screw','M4x10 Cap Screw','M4x10 Cap Screw',(#12266));
#12309=PRODUCT('Connecting link (1)','Connecting link (1)',
'Connecting link (1)',(#12266));
#12310=PRODUCT('Connecting link','Connecting link','Connecting link',
(#12266));
#12311=PRODUCT('Link bushing','Link bushing','Link bushing',(#12266));
#12312=PRODUCT('Link bushing (1)','Link bushing (1)','Link bushing (1)',(#12266));
#12313=PRESENTATION_STYLE_ASSIGNMENT((#12318));
#12314=PRESENTATION_STYLE_ASSIGNMENT((#12319));
#12315=PRESENTATION_STYLE_ASSIGNMENT((#12320));
#12316=PRESENTATION_STYLE_ASSIGNMENT((#12321));
#12317=PRESENTATION_STYLE_ASSIGNMENT((#12322));
#12318=SURFACE_STYLE_USAGE(.BOTH.,#12323);
#12319=SURFACE_STYLE_USAGE(.BOTH.,#12324);
#12320=SURFACE_STYLE_USAGE(.BOTH.,#12325);
#12321=SURFACE_STYLE_USAGE(.BOTH.,#12326);
#12322=SURFACE_STYLE_USAGE(.BOTH.,#12327);
#12323=SURFACE_SIDE_STYLE('',(#12328));
#12324=SURFACE_SIDE_STYLE('',(#12329));
#12325=SURFACE_SIDE_STYLE('',(#12330));
#12326=SURFACE_SIDE_STYLE('',(#12331));
#12327=SURFACE_SIDE_STYLE('',(#12332));
#12328=SURFACE_STYLE_FILL_AREA(#12333);
#12329=SURFACE_STYLE_FILL_AREA(#12334);
#12330=SURFACE_STYLE_FILL_AREA(#12335);
#12331=SURFACE_STYLE_FILL_AREA(#12336);
#12332=SURFACE_STYLE_FILL_AREA(#12337);
#12333=FILL_AREA_STYLE('Steel - Satin',(#12338));
#12334=FILL_AREA_STYLE('CAD Library Painted - Deep blue',(#12339));
#12335=FILL_AREA_STYLE('CAD Library Painted - Engineering blue',(#12340));
#12336=FILL_AREA_STYLE('CAD Library Painted - Steel gray',(#12341));
#12337=FILL_AREA_STYLE('CAD Library Painted - Graphite',(#12342));
#12338=FILL_AREA_STYLE_COLOUR('Steel - Satin',#12343);
#12339=FILL_AREA_STYLE_COLOUR('CAD Library Painted - Deep blue',#12344);
#12340=FILL_AREA_STYLE_COLOUR('CAD Library Painted - Engineering blue',
#12345);
#12341=FILL_AREA_STYLE_COLOUR('CAD Library Painted - Steel gray',#12346);
#12342=FILL_AREA_STYLE_COLOUR('CAD Library Painted - Graphite',#12347);
#12343=COLOUR_RGB('Steel - Satin',0.627450980392157,0.627450980392157,0.627450980392157);
#12344=COLOUR_RGB('CAD Library Painted - Deep blue',0.0784313725490196,
0.203921568627451,0.349019607843137);
#12345=COLOUR_RGB('CAD Library Painted - Engineering blue',0.12156862745098,
0.356862745098039,0.6);
#12346=COLOUR_RGB('CAD Library Painted - Steel gray',0.592156862745098,
0.631372549019608,0.67843137254902);
#12347=COLOUR_RGB('CAD Library Painted - Graphite',0.168627450980392,0.192156862745098,
0.231372549019608);
#12348=COLOUR_RGB('Dark Blue',0.08,0.2,0.34);
#12349=FILL_AREA_STYLE_COLOUR('',#12348);
#12350=FILL_AREA_STYLE('',(#12349));
#12351=SURFACE_STYLE_FILL_AREA(#12350);
#12352=SURFACE_SIDE_STYLE('',(#12351));
#12353=SURFACE_STYLE_USAGE(.BOTH.,#12352);
#12354=PRESENTATION_STYLE_ASSIGNMENT((#12353));
#12355=COLOUR_RGB('Light Blue',0.38,0.62,0.78);
#12356=FILL_AREA_STYLE_COLOUR('',#12355);
#12357=FILL_AREA_STYLE('',(#12356));
#12358=SURFACE_STYLE_FILL_AREA(#12357);
#12359=SURFACE_SIDE_STYLE('',(#12358));
#12360=SURFACE_STYLE_USAGE(.BOTH.,#12359);
#12361=PRESENTATION_STYLE_ASSIGNMENT((#12360));
#12362=COLOUR_RGB('Sky Blue',0.24,0.69,0.87);
#12363=FILL_AREA_STYLE_COLOUR('',#12362);
#12364=FILL_AREA_STYLE('',(#12363));
#12365=SURFACE_STYLE_FILL_AREA(#12364);
#12366=SURFACE_SIDE_STYLE('',(#12365));
#12367=SURFACE_STYLE_USAGE(.BOTH.,#12366);
#12368=PRESENTATION_STYLE_ASSIGNMENT((#12367));
#12369=COLOUR_RGB('Grey',0.48,0.52,0.57);
#12370=FILL_AREA_STYLE_COLOUR('',#12369);
#12371=FILL_AREA_STYLE('',(#12370));
#12372=SURFACE_STYLE_FILL_AREA(#12371);
#12373=SURFACE_SIDE_STYLE('',(#12372));
#12374=SURFACE_STYLE_USAGE(.BOTH.,#12373);
#12375=PRESENTATION_STYLE_ASSIGNMENT((#12374));
#12376=COLOUR_RGB('Black',0.12,0.14,0.17);
#12377=FILL_AREA_STYLE_COLOUR('',#12376);
#12378=FILL_AREA_STYLE('',(#12377));
#12379=SURFACE_STYLE_FILL_AREA(#12378);
#12380=SURFACE_SIDE_STYLE('',(#12379));
#12381=SURFACE_STYLE_USAGE(.BOTH.,#12380);
#12382=PRESENTATION_STYLE_ASSIGNMENT((#12381));
#12383=COLOUR_RGB('Off White',0.89,0.88,0.83);
#12384=FILL_AREA_STYLE_COLOUR('',#12383);
#12385=FILL_AREA_STYLE('',(#12384));
#12386=SURFACE_STYLE_FILL_AREA(#12385);
#12387=SURFACE_SIDE_STYLE('',(#12386));
#12388=SURFACE_STYLE_USAGE(.BOTH.,#12387);
#12389=PRESENTATION_STYLE_ASSIGNMENT((#12388));
ENDSEC;
END-ISO-10303-21;
